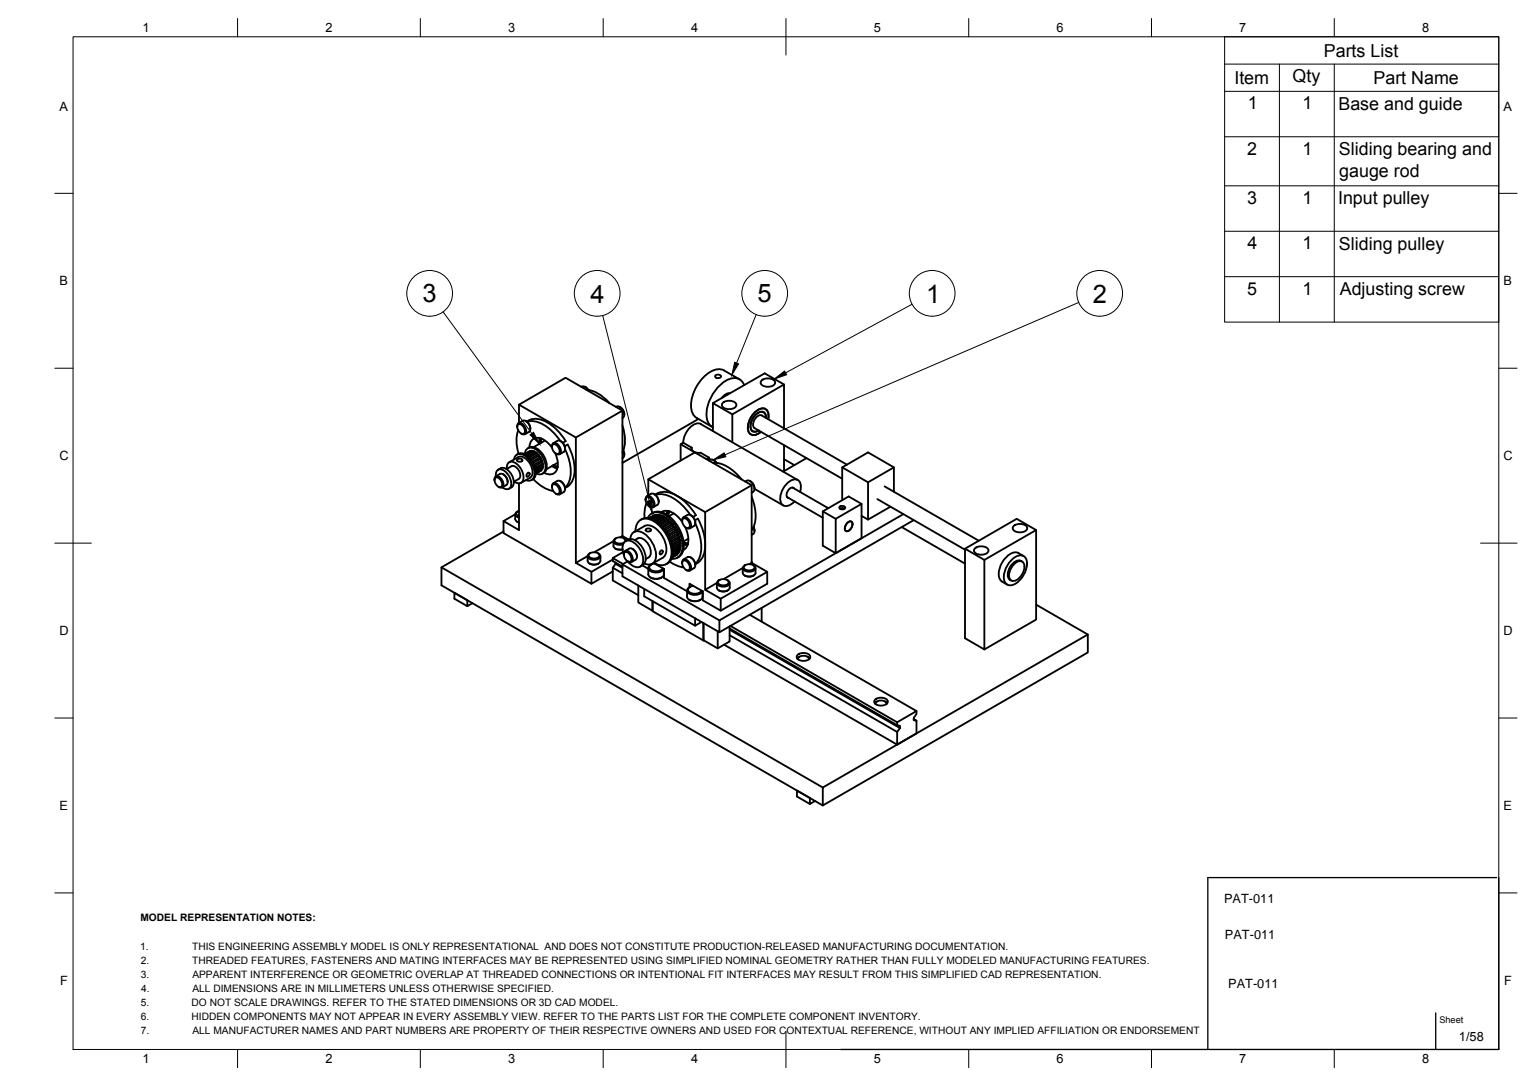
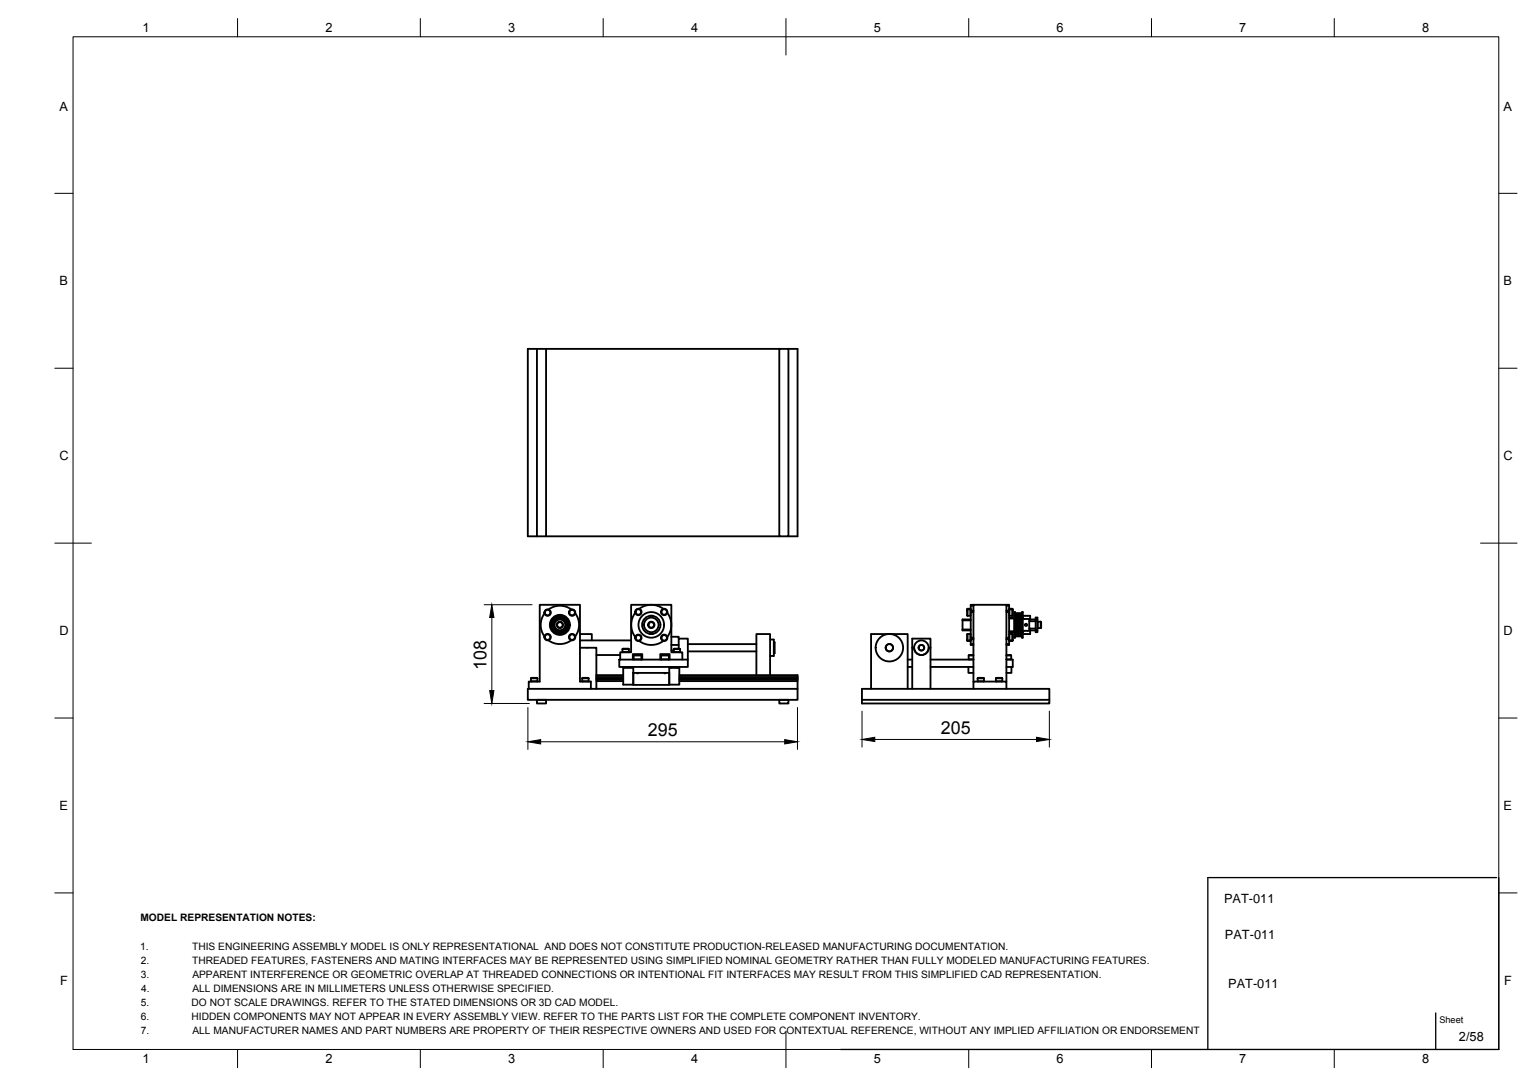
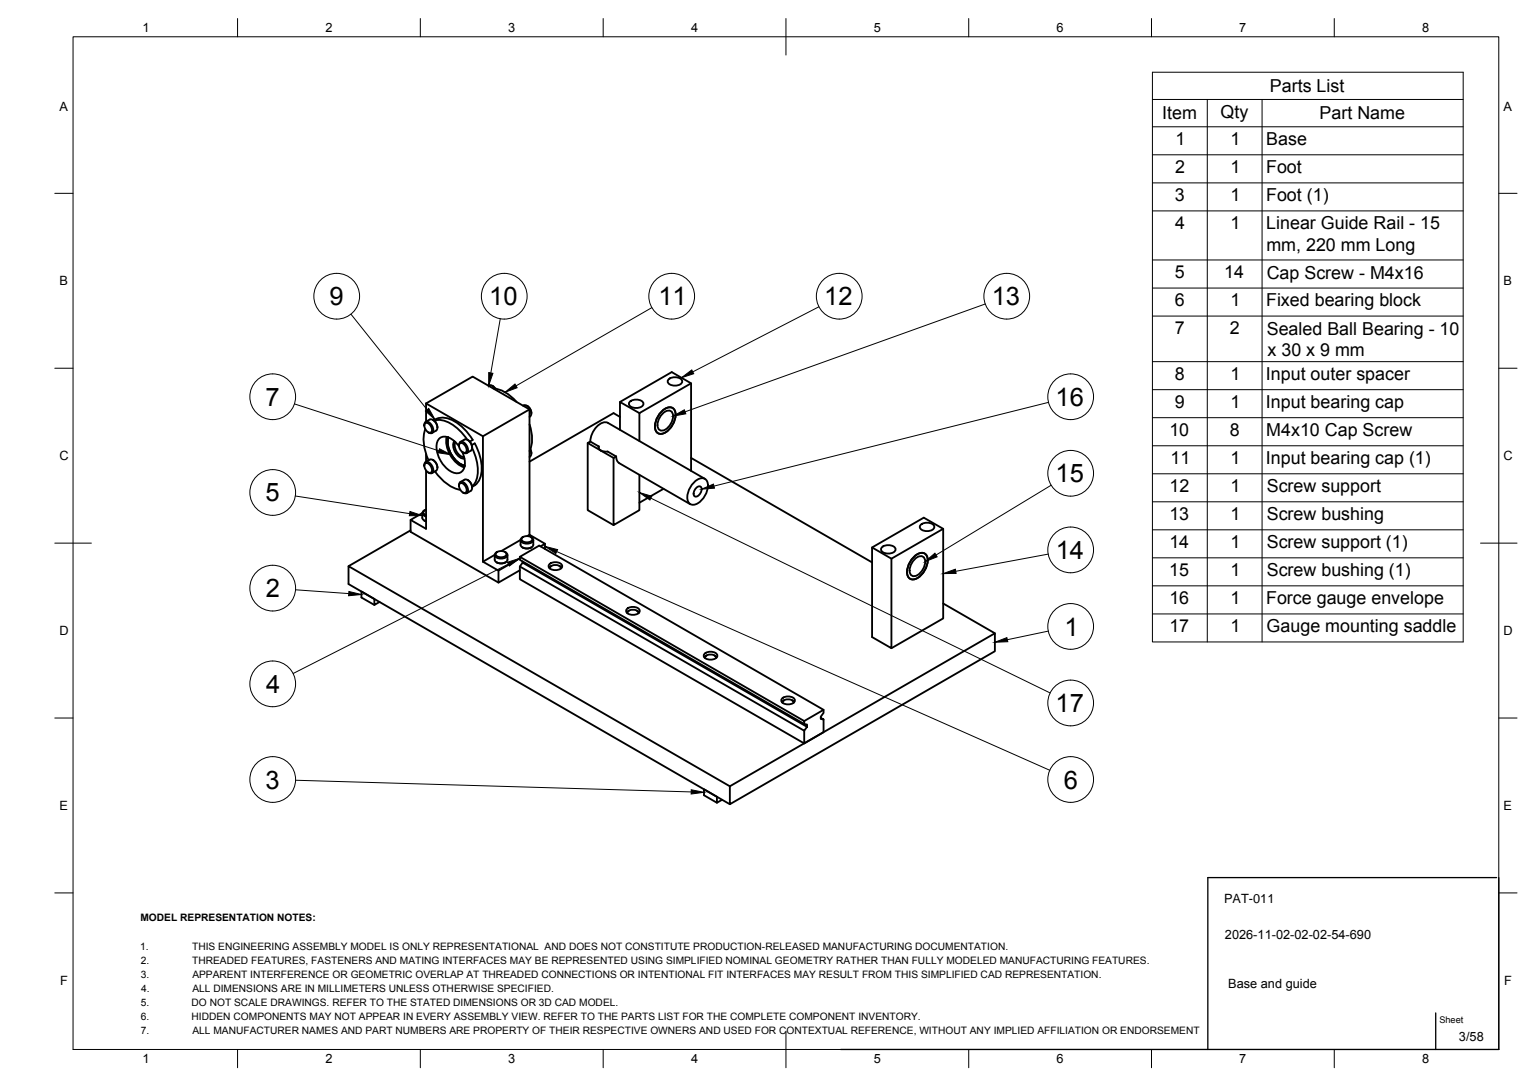
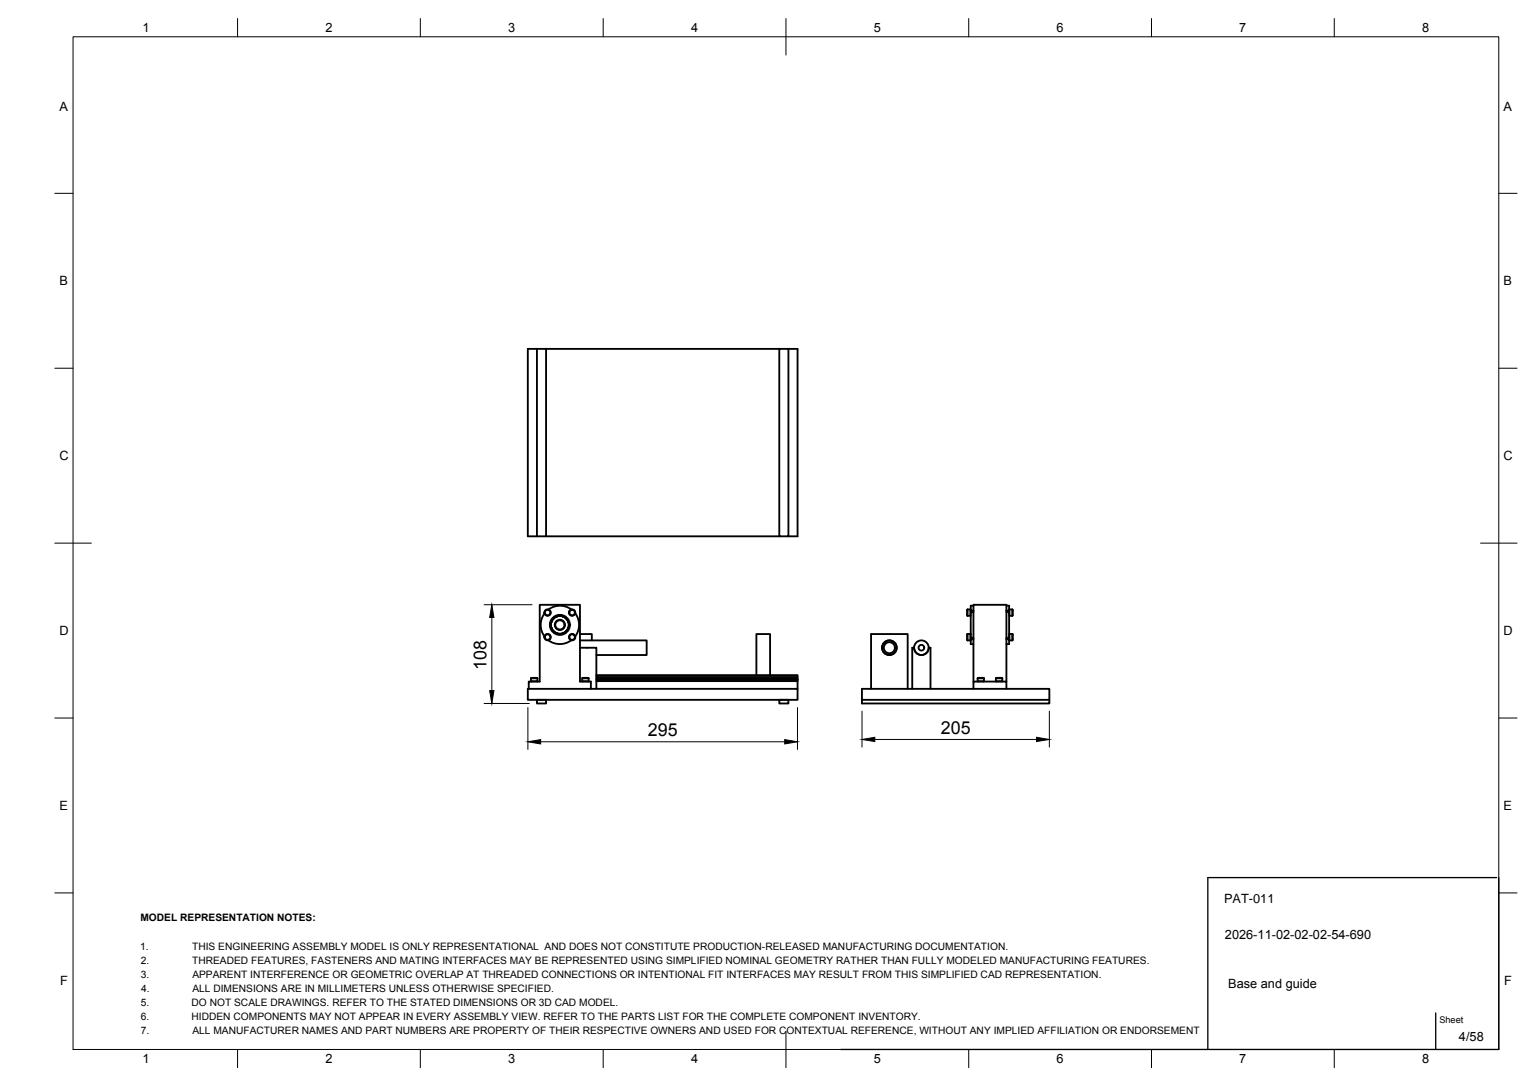
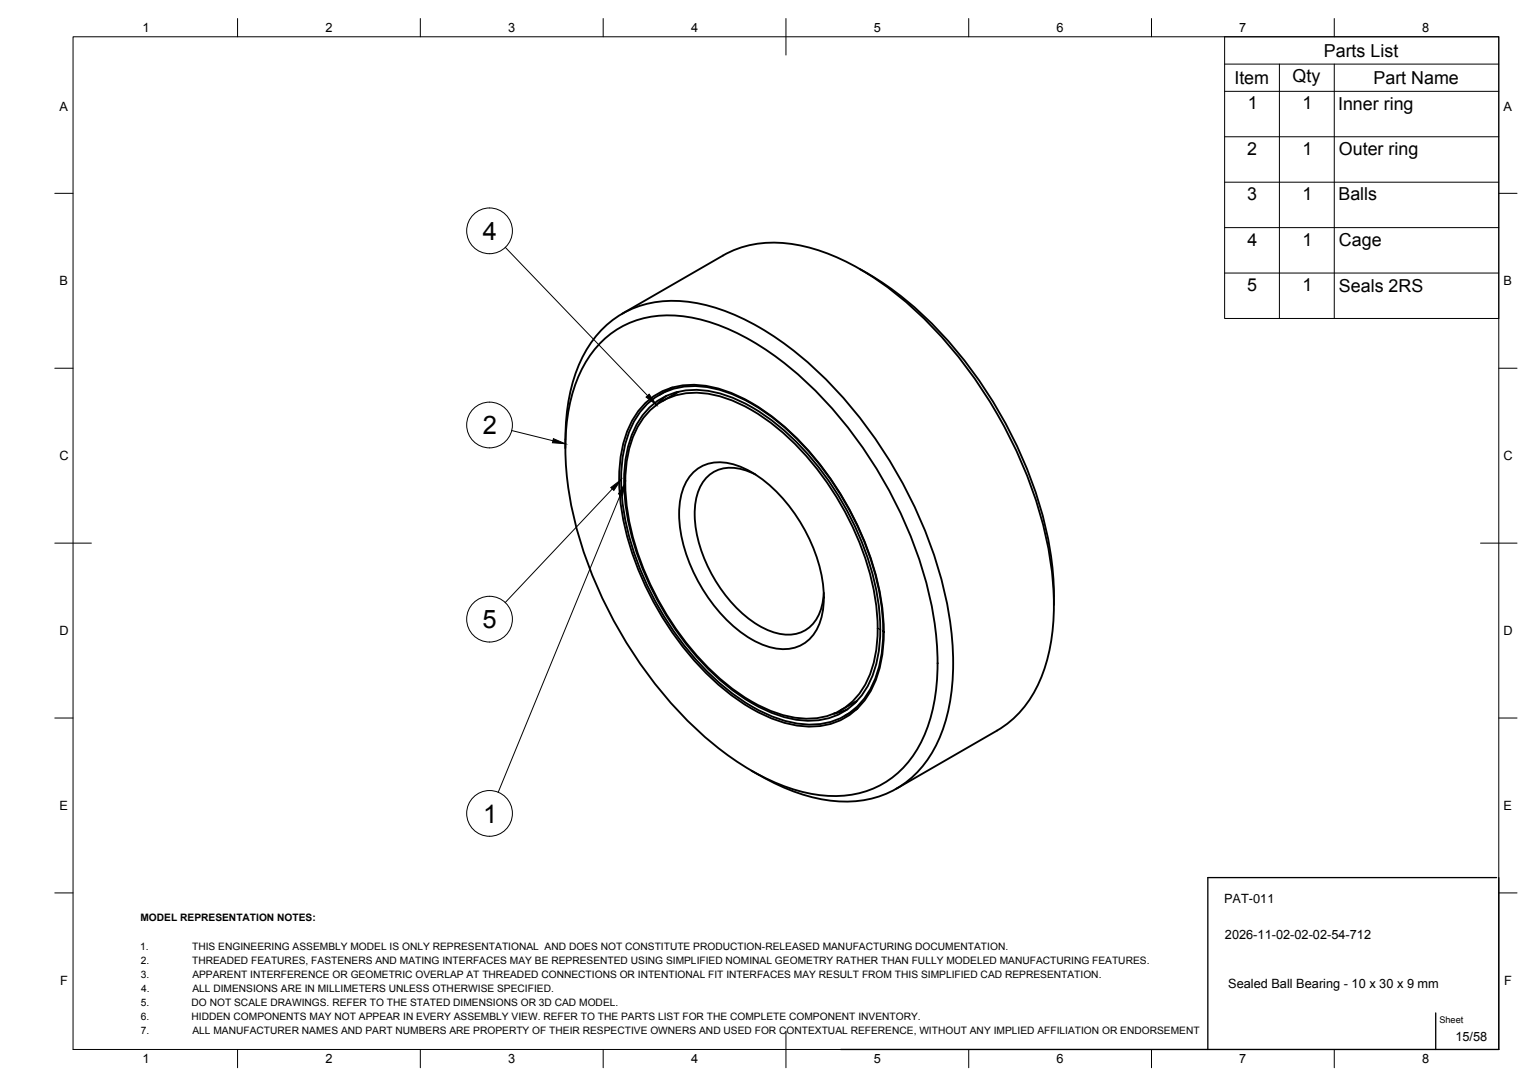
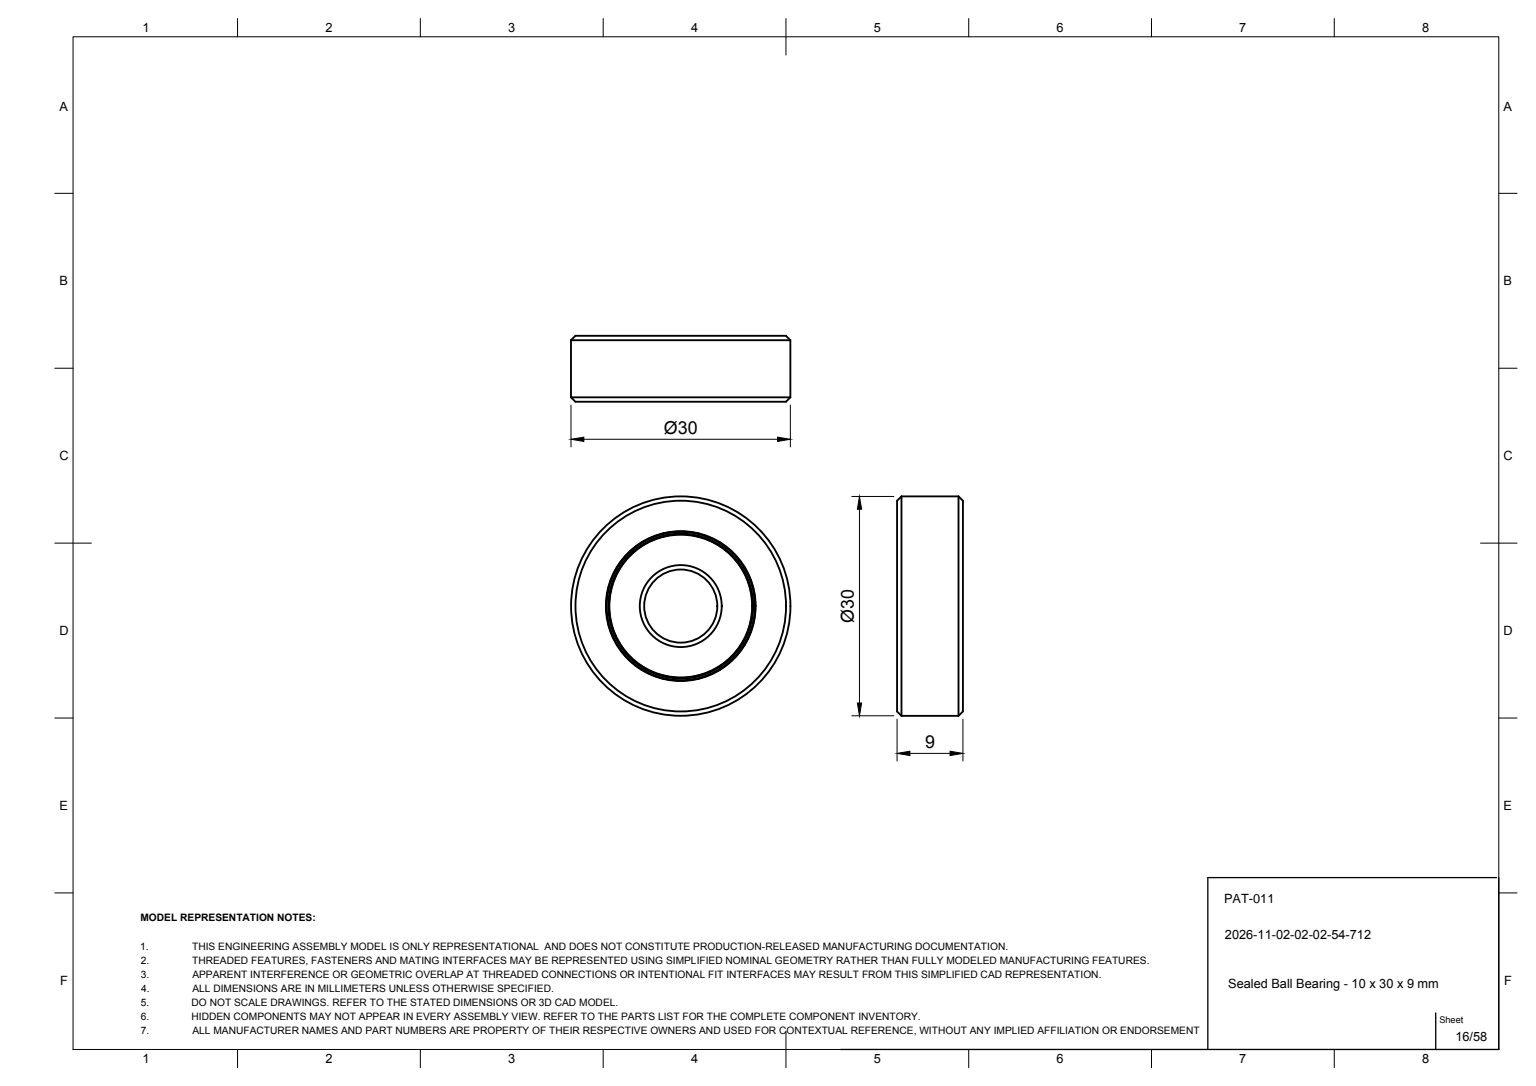
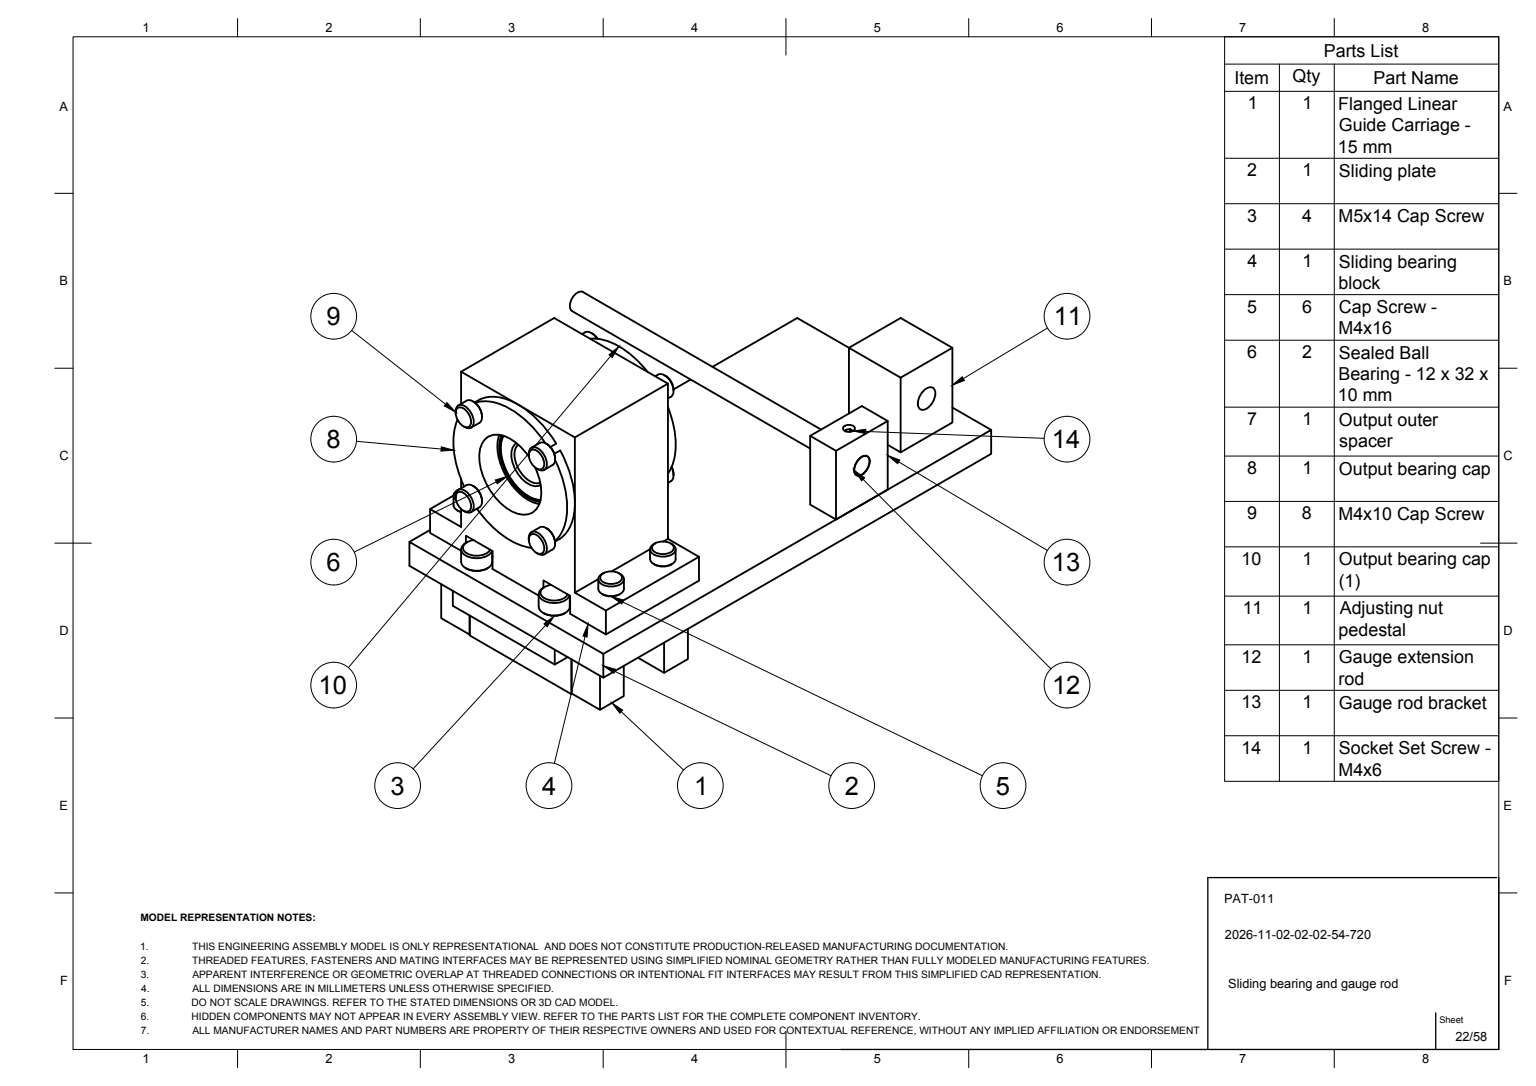
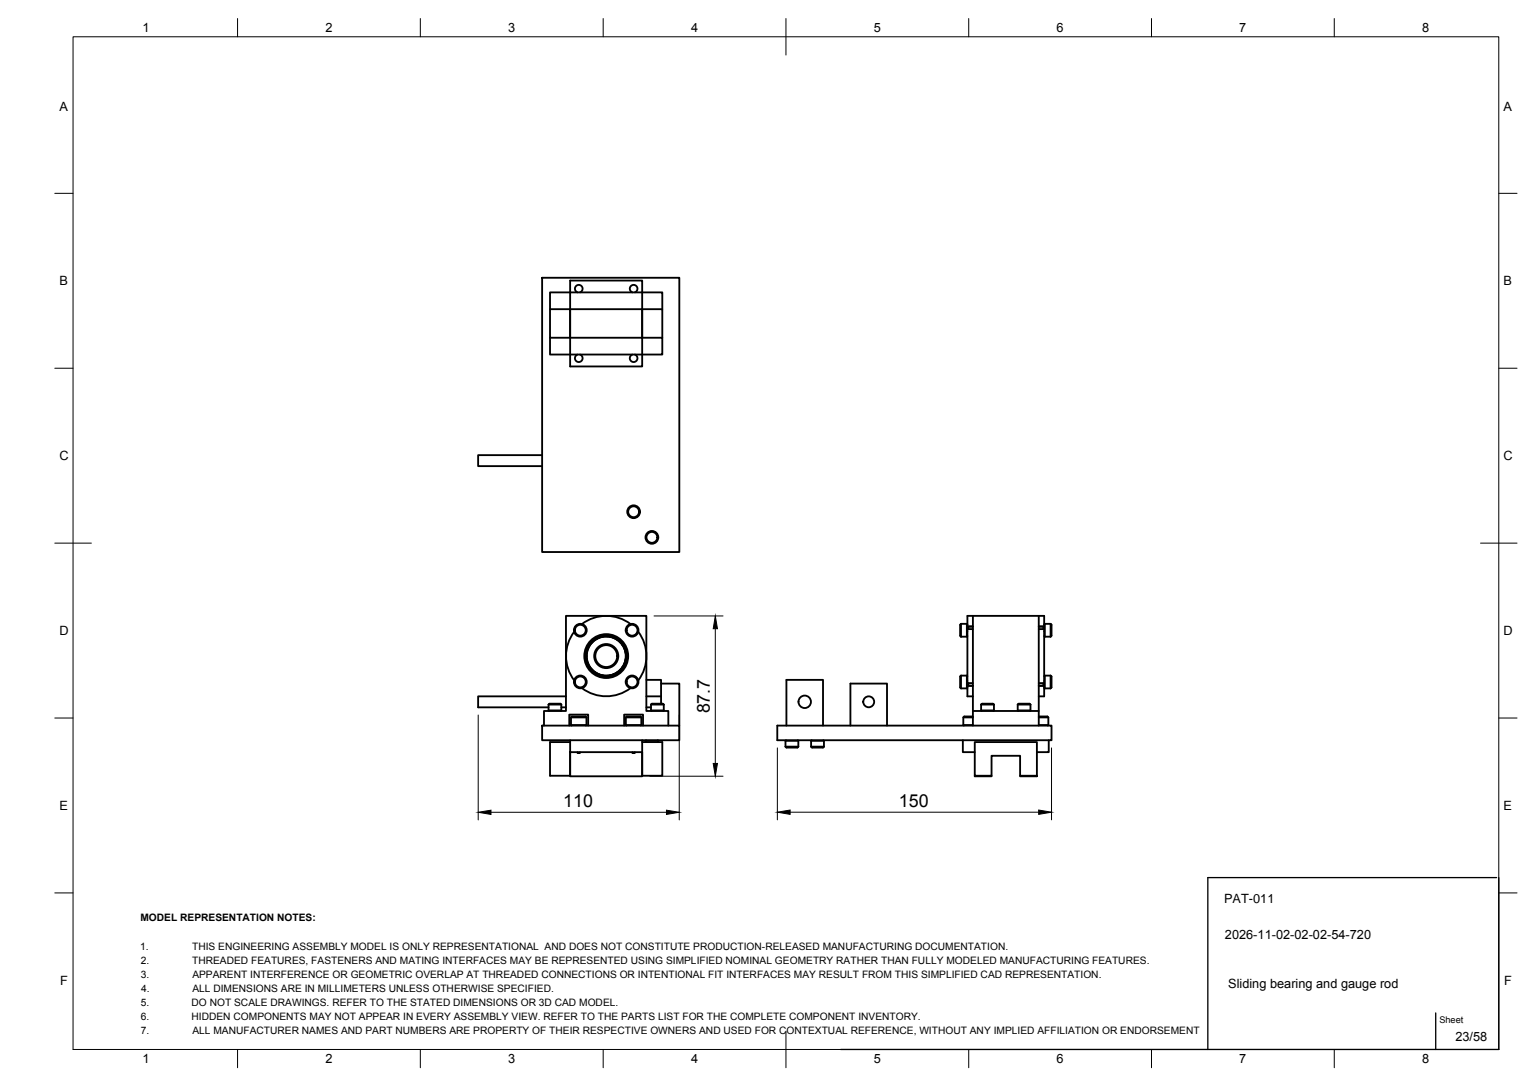
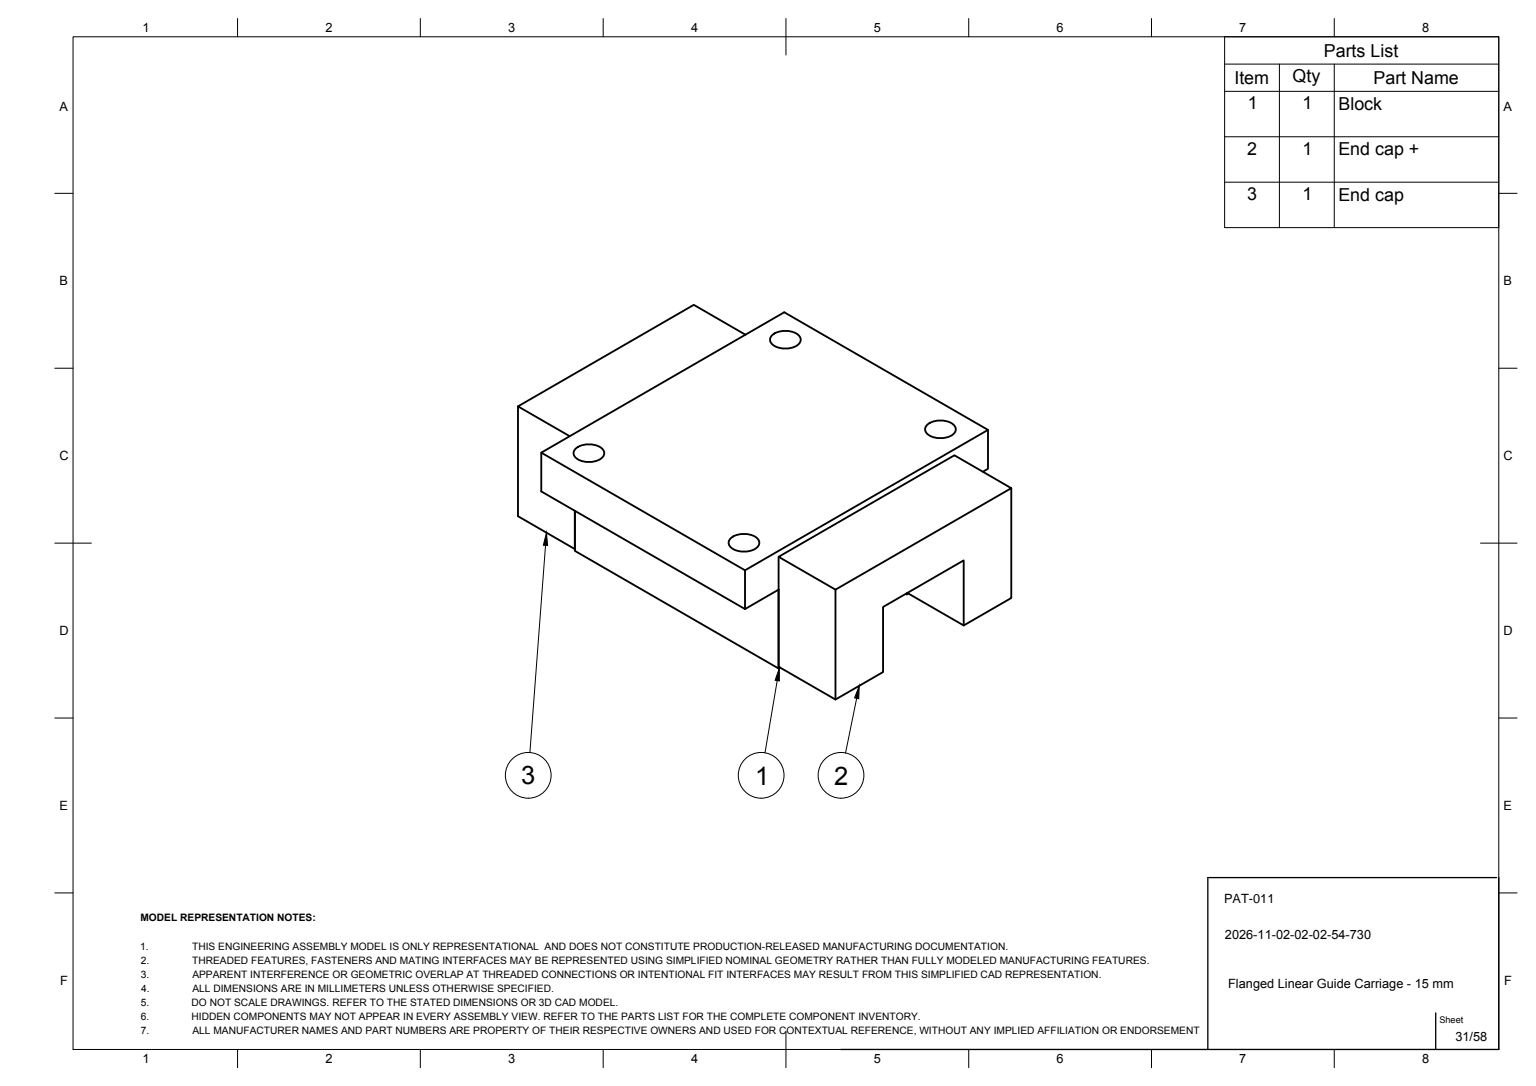
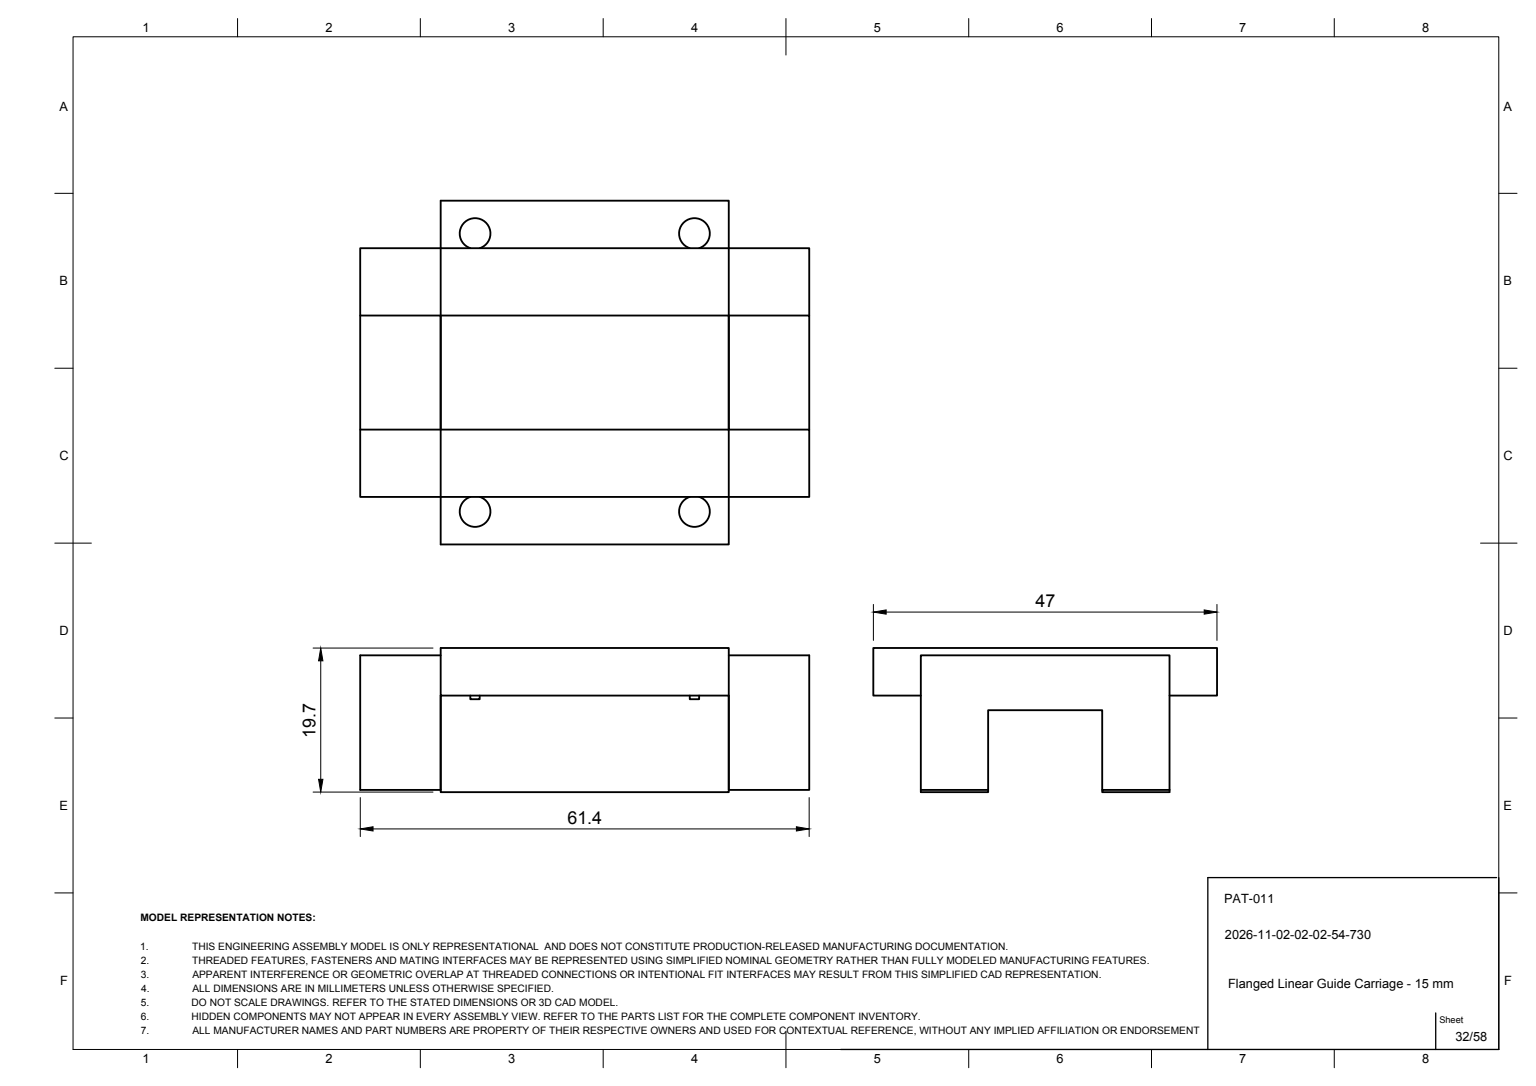
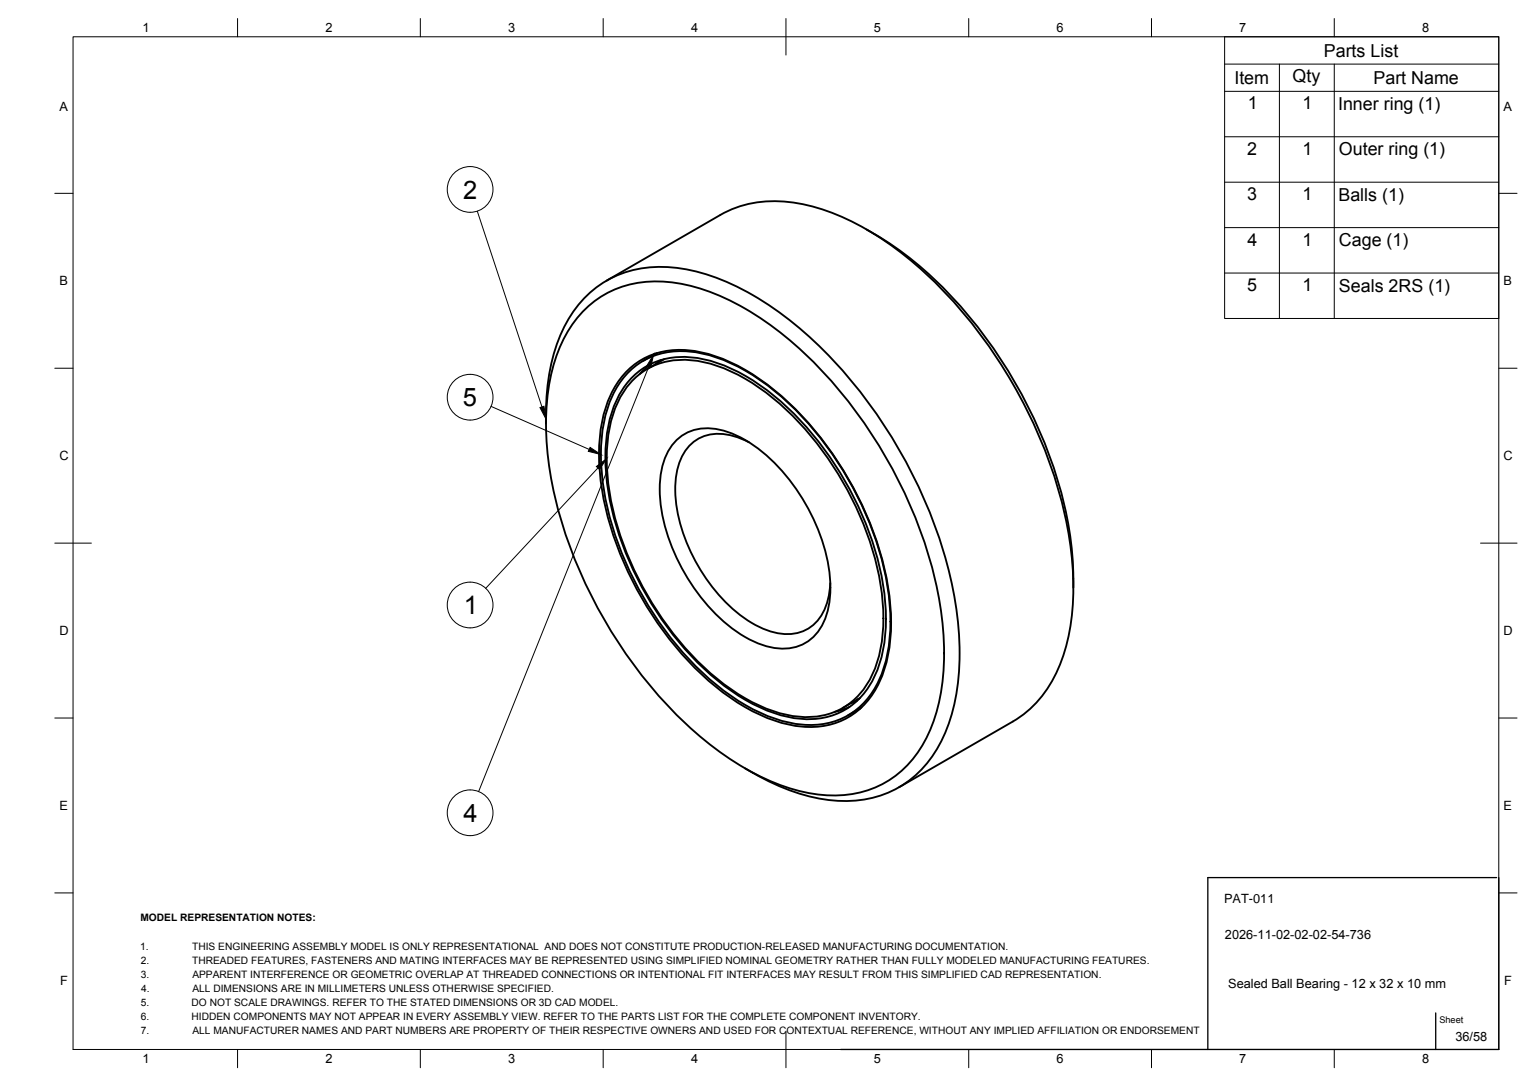
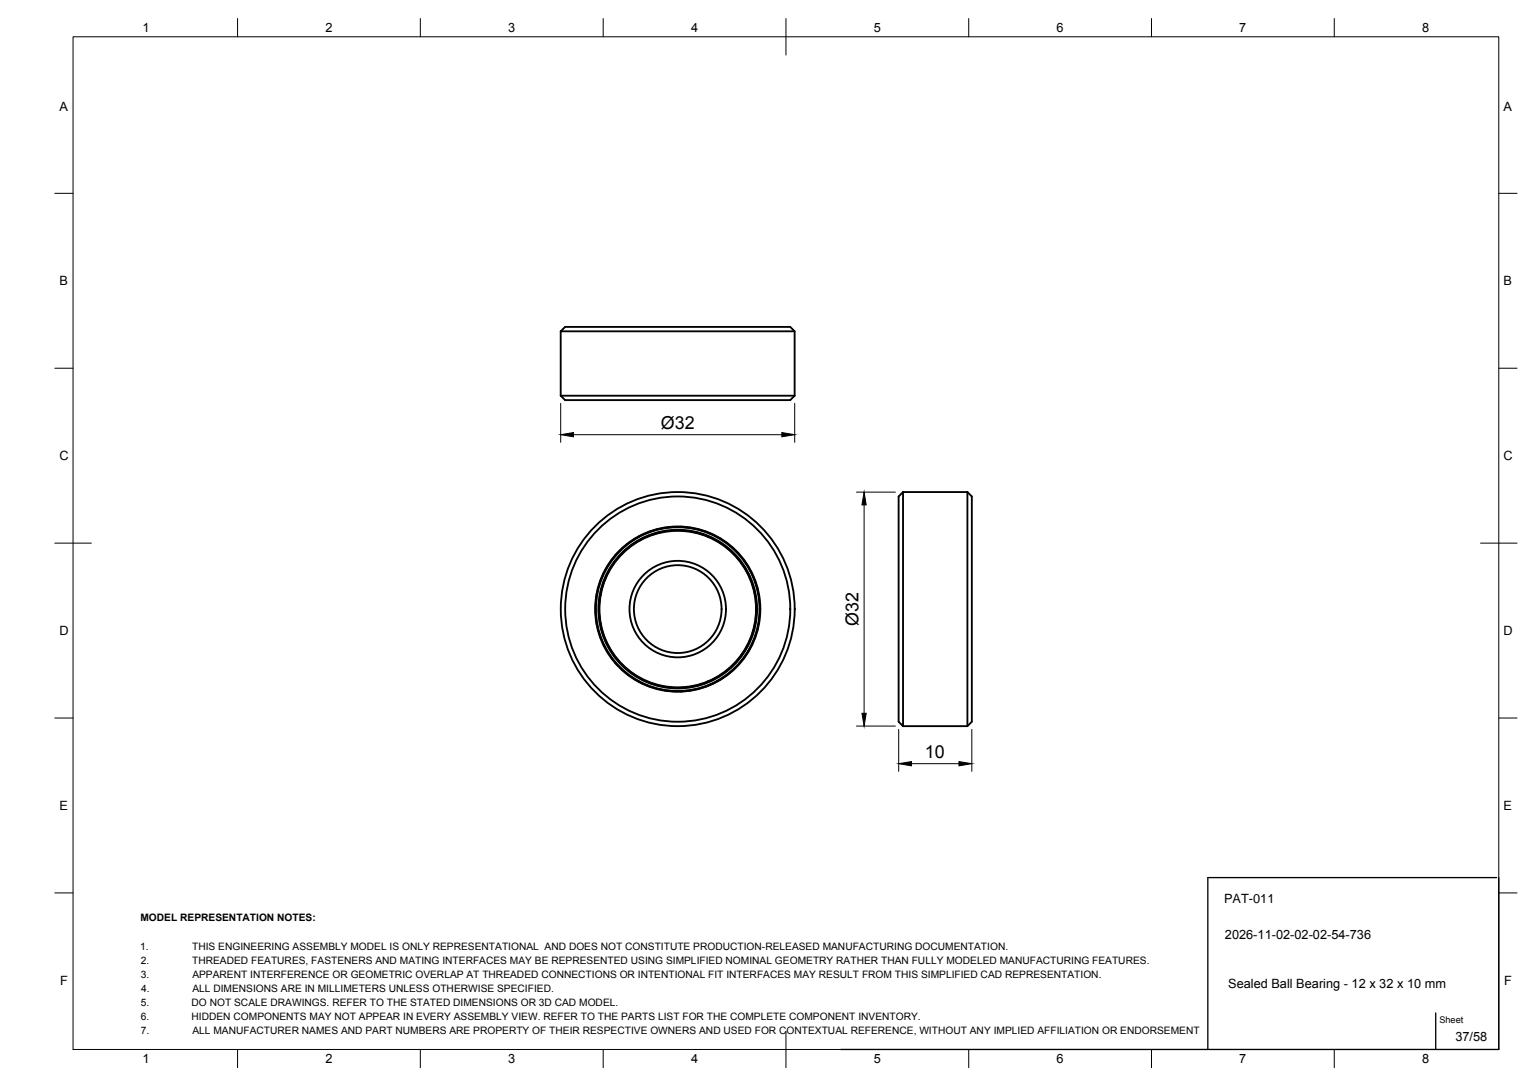
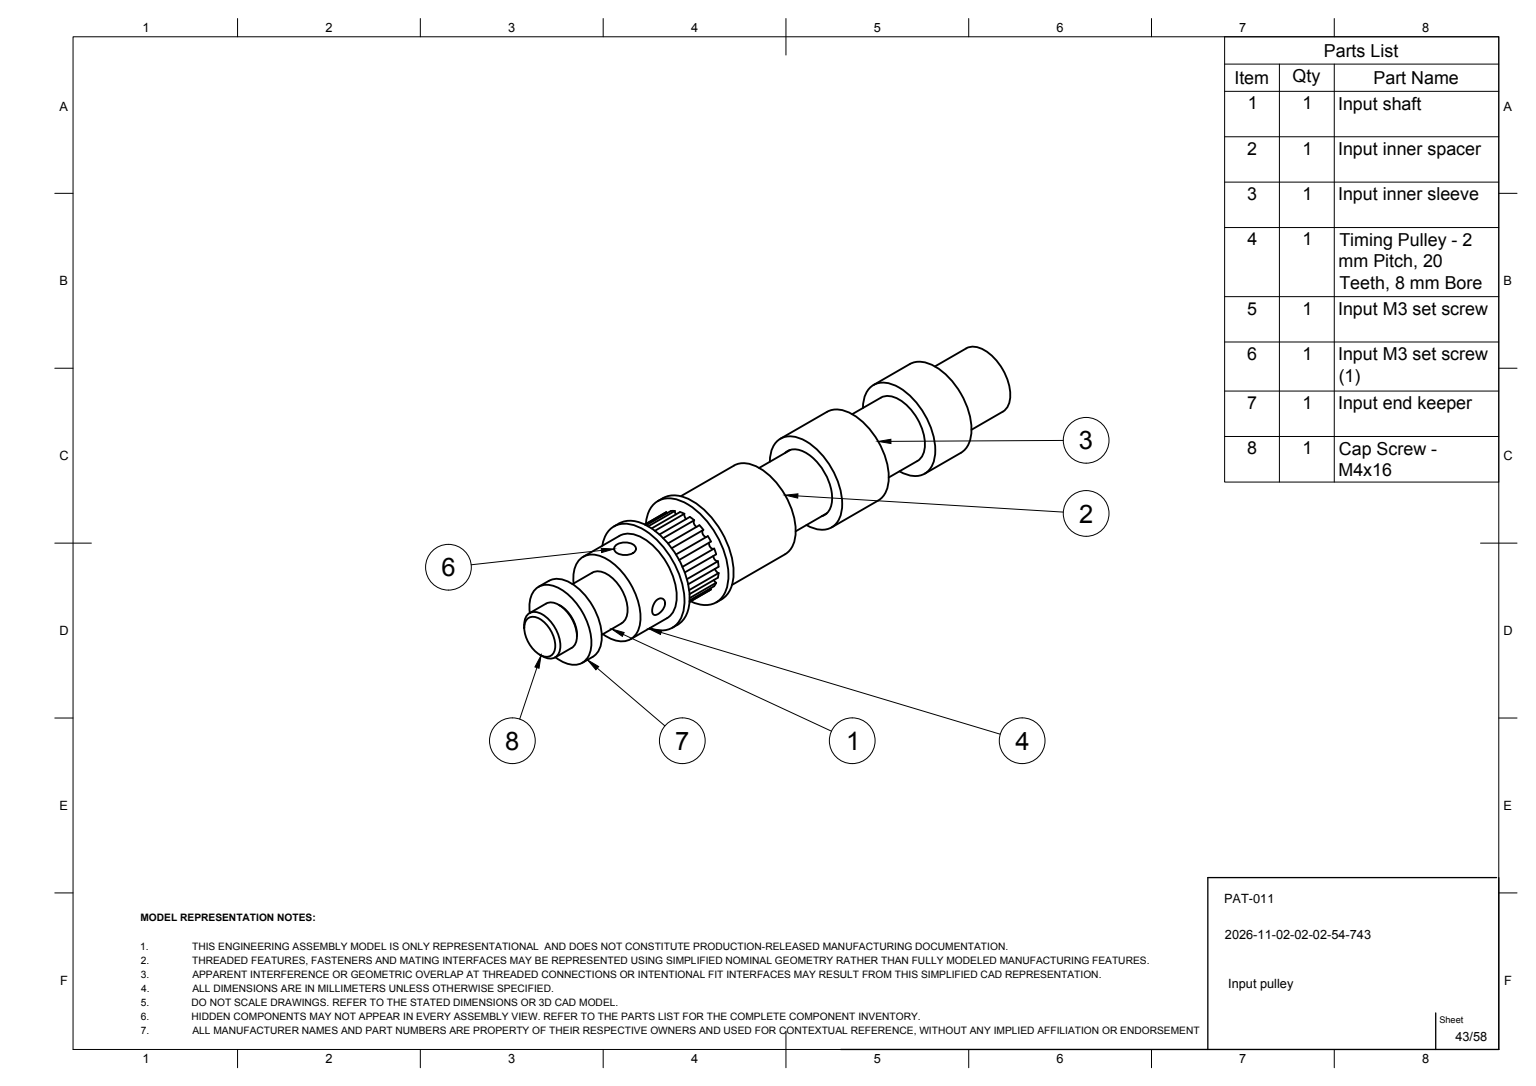
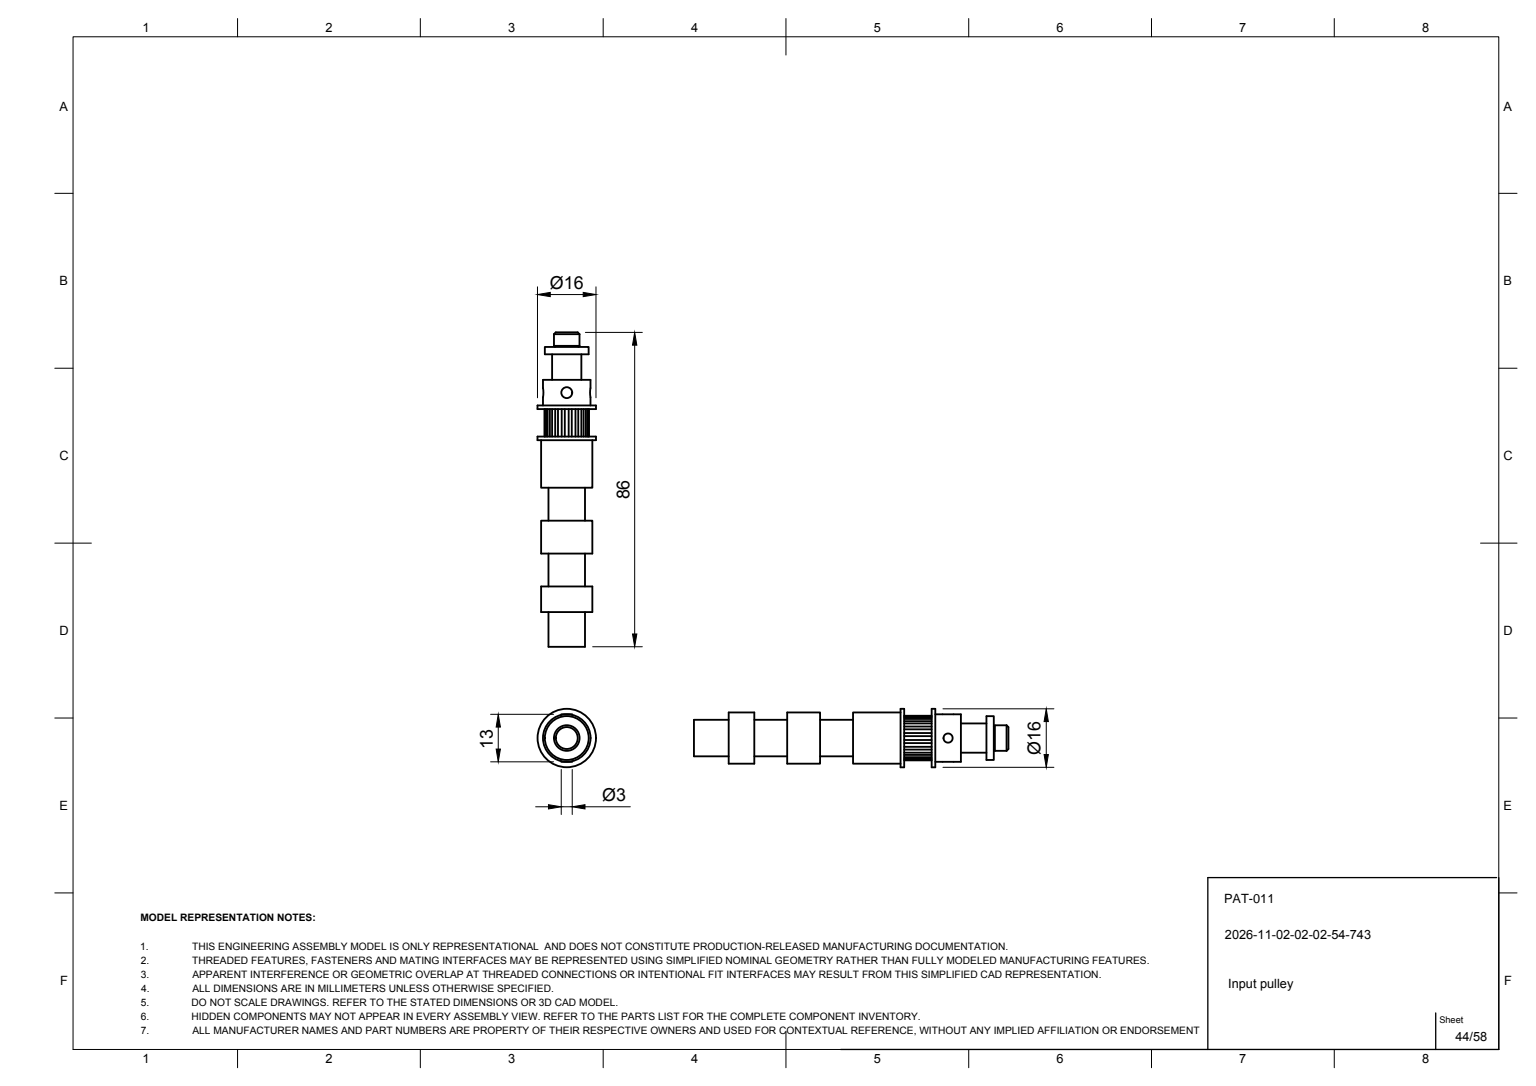
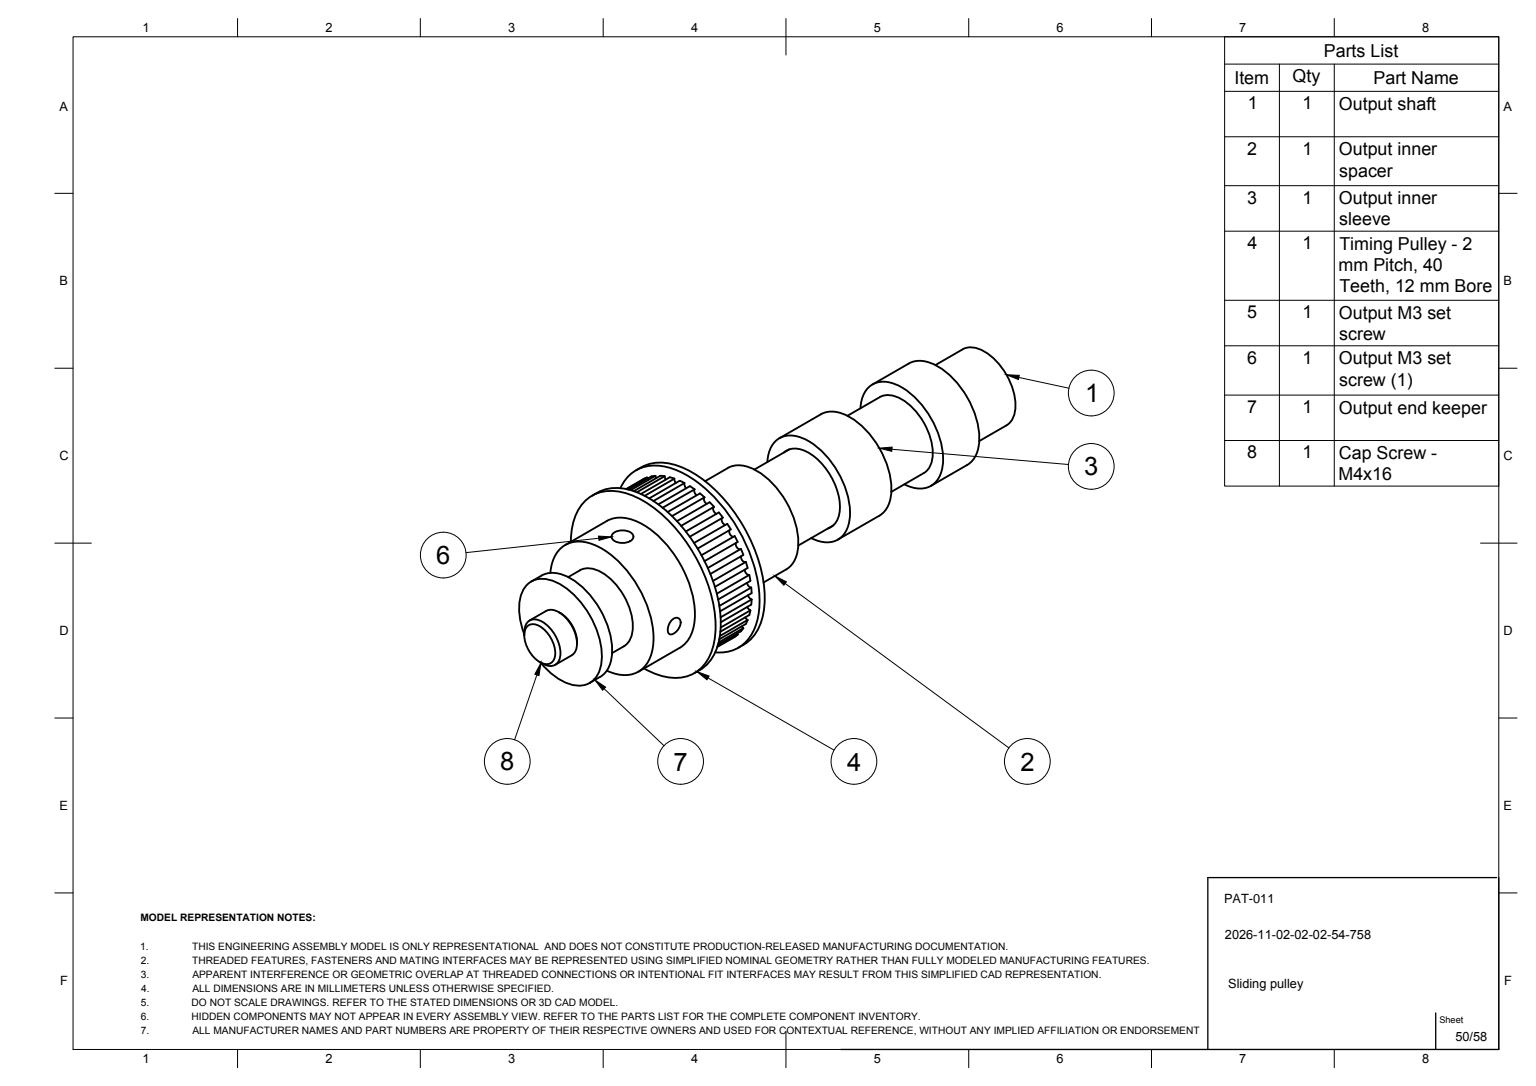
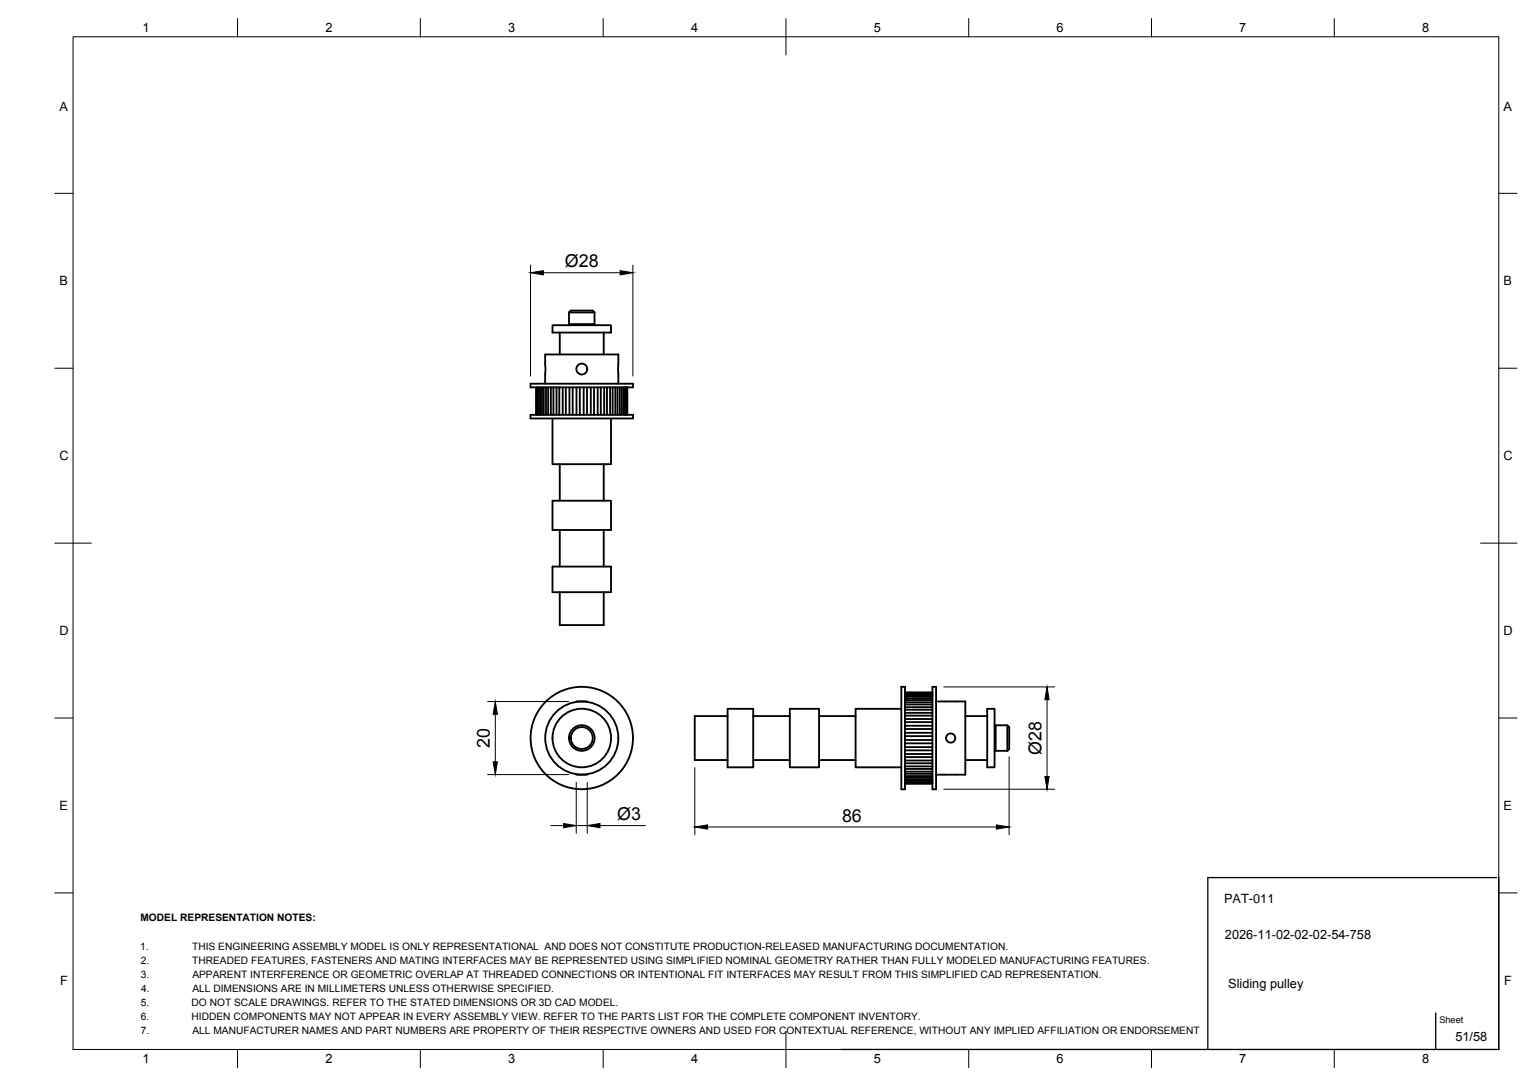
ISO-10303-21;
HEADER;
/* Generated by software containing ST-Developer
 * from STEP Tools, Inc. (www.steptools.com) 
 */

FILE_DESCRIPTION(
/* description */ ('Belt tension measurement rig'),
/* implementation_level */ '2;1');

FILE_NAME(
/* name */ 'PAT-011',
/* time_stamp */ '2026-10-28T03:24:44-07:00',
/* author */ (''),
/* organization */ (''),
/* preprocessor_version */ 'ST-DEVELOPER v20.2',
/* originating_system */ 'Autodesk Translation Framework v15.17.0.0',
/* authorisation */ '');

FILE_SCHEMA (('AUTOMOTIVE_DESIGN { 1 0 10303 214 3 1 1 }'));
ENDSEC;

DATA;
#10=MECHANICAL_DESIGN_GEOMETRIC_PRESENTATION_REPRESENTATION('',(#692,#693,
#694,#695,#696,#697,#698,#699,#700,#701,#702,#703,#704,#705,#706,#707,#708,
#709,#710,#711,#712,#713,#714,#715,#716,#717,#718,#719,#720,#721,#722,#723,
#724,#725,#726,#727,#728,#729,#730,#731,#732,#733,#734,#735,#736,#737,#738,
#739,#740,#741,#742,#743,#744,#745,#746,#747,#748,#749,#750,#751,#752,#753,
#754,#755,#756,#757,#758,#759,#760,#761),#23587);
#11=ORIENTED_CLOSED_SHELL('',*,#12235,.F.);
#12=ORIENTED_CLOSED_SHELL('',*,#12249,.F.);
#13=ORIENTED_CLOSED_SHELL('',*,#12266,.F.);
#14=BREP_WITH_VOIDS('Body1',#12236,(#11));
#15=BREP_WITH_VOIDS('Body1',#12250,(#12));
#16=BREP_WITH_VOIDS('Body1',#12265,(#13));
#17=ITEM_DEFINED_TRANSFORMATION($,$,#13222,#13350);
#18=ITEM_DEFINED_TRANSFORMATION($,$,#13242,#13351);
#19=ITEM_DEFINED_TRANSFORMATION($,$,#13262,#13352);
#20=ITEM_DEFINED_TRANSFORMATION($,$,#13279,#13353);
#21=ITEM_DEFINED_TRANSFORMATION($,$,#13333,#13354);
#22=ITEM_DEFINED_TRANSFORMATION($,$,#13565,#13626);
#23=ITEM_DEFINED_TRANSFORMATION($,$,#13604,#13627);
#24=ITEM_DEFINED_TRANSFORMATION($,$,#13615,#13628);
#25=ITEM_DEFINED_TRANSFORMATION($,$,#13654,#13776);
#26=ITEM_DEFINED_TRANSFORMATION($,$,#13674,#13777);
#27=ITEM_DEFINED_TRANSFORMATION($,$,#13694,#13778);
#28=ITEM_DEFINED_TRANSFORMATION($,$,#13709,#13779);
#29=ITEM_DEFINED_TRANSFORMATION($,$,#13759,#13780);
#30=ITEM_DEFINED_TRANSFORMATION($,$,#12878,#14359);
#31=ITEM_DEFINED_TRANSFORMATION($,$,#12941,#14360);
#32=ITEM_DEFINED_TRANSFORMATION($,$,#12948,#14361);
#33=ITEM_DEFINED_TRANSFORMATION($,$,#12955,#14362);
#34=ITEM_DEFINED_TRANSFORMATION($,$,#12993,#14363);
#35=ITEM_DEFINED_TRANSFORMATION($,$,#13002,#14364);
#36=ITEM_DEFINED_TRANSFORMATION($,$,#13036,#14365);
#37=ITEM_DEFINED_TRANSFORMATION($,$,#13070,#14366);
#38=ITEM_DEFINED_TRANSFORMATION($,$,#13094,#14367);
#39=ITEM_DEFINED_TRANSFORMATION($,$,#13103,#14368);
#40=ITEM_DEFINED_TRANSFORMATION($,$,#13127,#14369);
#41=ITEM_DEFINED_TRANSFORMATION($,$,#13136,#14370);
#42=ITEM_DEFINED_TRANSFORMATION($,$,#13145,#14371);
#43=ITEM_DEFINED_TRANSFORMATION($,$,#13178,#14372);
#44=ITEM_DEFINED_TRANSFORMATION($,$,#14333,#14373);
#45=ITEM_DEFINED_TRANSFORMATION($,$,#14333,#14374);
#46=ITEM_DEFINED_TRANSFORMATION($,$,#14333,#14375);
#47=ITEM_DEFINED_TRANSFORMATION($,$,#14333,#14376);
#48=ITEM_DEFINED_TRANSFORMATION($,$,#14333,#14377);
#49=ITEM_DEFINED_TRANSFORMATION($,$,#14333,#14378);
#50=ITEM_DEFINED_TRANSFORMATION($,$,#14333,#14379);
#51=ITEM_DEFINED_TRANSFORMATION($,$,#14333,#14380);
#52=ITEM_DEFINED_TRANSFORMATION($,$,#13221,#14381);
#53=ITEM_DEFINED_TRANSFORMATION($,$,#13221,#14382);
#54=ITEM_DEFINED_TRANSFORMATION($,$,#13781,#14383);
#55=ITEM_DEFINED_TRANSFORMATION($,$,#13781,#14384);
#56=ITEM_DEFINED_TRANSFORMATION($,$,#13781,#14385);
#57=ITEM_DEFINED_TRANSFORMATION($,$,#13781,#14386);
#58=ITEM_DEFINED_TRANSFORMATION($,$,#13781,#14387);
#59=ITEM_DEFINED_TRANSFORMATION($,$,#13781,#14388);
#60=ITEM_DEFINED_TRANSFORMATION($,$,#13781,#14389);
#61=ITEM_DEFINED_TRANSFORMATION($,$,#13781,#14390);
#62=ITEM_DEFINED_TRANSFORMATION($,$,#14333,#14391);
#63=ITEM_DEFINED_TRANSFORMATION($,$,#14333,#14392);
#64=ITEM_DEFINED_TRANSFORMATION($,$,#14333,#14393);
#65=ITEM_DEFINED_TRANSFORMATION($,$,#14333,#14394);
#66=ITEM_DEFINED_TRANSFORMATION($,$,#14333,#14395);
#67=ITEM_DEFINED_TRANSFORMATION($,$,#14333,#14396);
#68=ITEM_DEFINED_TRANSFORMATION($,$,#13806,#14397);
#69=ITEM_DEFINED_TRANSFORMATION($,$,#13828,#14398);
#70=ITEM_DEFINED_TRANSFORMATION($,$,#13841,#14399);
#71=ITEM_DEFINED_TRANSFORMATION($,$,#13850,#14400);
#72=ITEM_DEFINED_TRANSFORMATION($,$,#13856,#14401);
#73=ITEM_DEFINED_TRANSFORMATION($,$,#13862,#14402);
#74=ITEM_DEFINED_TRANSFORMATION($,$,#13871,#14403);
#75=ITEM_DEFINED_TRANSFORMATION($,$,#14333,#14404);
#76=ITEM_DEFINED_TRANSFORMATION($,$,#14014,#14405);
#77=ITEM_DEFINED_TRANSFORMATION($,$,#14032,#14406);
#78=ITEM_DEFINED_TRANSFORMATION($,$,#14041,#14407);
#79=ITEM_DEFINED_TRANSFORMATION($,$,#14050,#14408);
#80=ITEM_DEFINED_TRANSFORMATION($,$,#14056,#14409);
#81=ITEM_DEFINED_TRANSFORMATION($,$,#14062,#14410);
#82=ITEM_DEFINED_TRANSFORMATION($,$,#14071,#14411);
#83=ITEM_DEFINED_TRANSFORMATION($,$,#14333,#14412);
#84=ITEM_DEFINED_TRANSFORMATION($,$,#13356,#14479);
#85=ITEM_DEFINED_TRANSFORMATION($,$,#13393,#14480);
#86=ITEM_DEFINED_TRANSFORMATION($,$,#13447,#14481);
#87=ITEM_DEFINED_TRANSFORMATION($,$,#13456,#14482);
#88=ITEM_DEFINED_TRANSFORMATION($,$,#13490,#14483);
#89=ITEM_DEFINED_TRANSFORMATION($,$,#13524,#14484);
#90=ITEM_DEFINED_TRANSFORMATION($,$,#13542,#14485);
#91=ITEM_DEFINED_TRANSFORMATION($,$,#13548,#14486);
#92=ITEM_DEFINED_TRANSFORMATION($,$,#13564,#14487);
#93=ITEM_DEFINED_TRANSFORMATION($,$,#13629,#14488);
#94=ITEM_DEFINED_TRANSFORMATION($,$,#13629,#14489);
#95=ITEM_DEFINED_TRANSFORMATION($,$,#13629,#14490);
#96=ITEM_DEFINED_TRANSFORMATION($,$,#13629,#14491);
#97=ITEM_DEFINED_TRANSFORMATION($,$,#14333,#14492);
#98=ITEM_DEFINED_TRANSFORMATION($,$,#14333,#14493);
#99=ITEM_DEFINED_TRANSFORMATION($,$,#14333,#14494);
#100=ITEM_DEFINED_TRANSFORMATION($,$,#14333,#14495);
#101=ITEM_DEFINED_TRANSFORMATION($,$,#13653,#14496);
#102=ITEM_DEFINED_TRANSFORMATION($,$,#13653,#14497);
#103=ITEM_DEFINED_TRANSFORMATION($,$,#13781,#14498);
#104=ITEM_DEFINED_TRANSFORMATION($,$,#13781,#14499);
#105=ITEM_DEFINED_TRANSFORMATION($,$,#13781,#14500);
#106=ITEM_DEFINED_TRANSFORMATION($,$,#13781,#14501);
#107=ITEM_DEFINED_TRANSFORMATION($,$,#13781,#14502);
#108=ITEM_DEFINED_TRANSFORMATION($,$,#13781,#14503);
#109=ITEM_DEFINED_TRANSFORMATION($,$,#13781,#14504);
#110=ITEM_DEFINED_TRANSFORMATION($,$,#13781,#14505);
#111=ITEM_DEFINED_TRANSFORMATION($,$,#14333,#14506);
#112=ITEM_DEFINED_TRANSFORMATION($,$,#14333,#14507);
#113=ITEM_DEFINED_TRANSFORMATION($,$,#14462,#14508);
#114=ITEM_DEFINED_TRANSFORMATION($,$,#14414,#14509);
#115=ITEM_DEFINED_TRANSFORMATION($,$,#14448,#14510);
#116=ITEM_DEFINED_TRANSFORMATION($,$,#14462,#14511);
#117=ITEM_DEFINED_TRANSFORMATION($,$,#12877,#14512);
#118=ITEM_DEFINED_TRANSFORMATION($,$,#13355,#14513);
#119=ITEM_DEFINED_TRANSFORMATION($,$,#13805,#14514);
#120=ITEM_DEFINED_TRANSFORMATION($,$,#14013,#14515);
#121=ITEM_DEFINED_TRANSFORMATION($,$,#14413,#14516);
#122=(
REPRESENTATION_RELATIONSHIP($,$,#23842,#23841)
REPRESENTATION_RELATIONSHIP_WITH_TRANSFORMATION(#17)
SHAPE_REPRESENTATION_RELATIONSHIP()
);
#123=(
REPRESENTATION_RELATIONSHIP($,$,#23843,#23841)
REPRESENTATION_RELATIONSHIP_WITH_TRANSFORMATION(#18)
SHAPE_REPRESENTATION_RELATIONSHIP()
);
#124=(
REPRESENTATION_RELATIONSHIP($,$,#23844,#23841)
REPRESENTATION_RELATIONSHIP_WITH_TRANSFORMATION(#19)
SHAPE_REPRESENTATION_RELATIONSHIP()
);
#125=(
REPRESENTATION_RELATIONSHIP($,$,#23845,#23841)
REPRESENTATION_RELATIONSHIP_WITH_TRANSFORMATION(#20)
SHAPE_REPRESENTATION_RELATIONSHIP()
);
#126=(
REPRESENTATION_RELATIONSHIP($,$,#23846,#23841)
REPRESENTATION_RELATIONSHIP_WITH_TRANSFORMATION(#21)
SHAPE_REPRESENTATION_RELATIONSHIP()
);
#127=(
REPRESENTATION_RELATIONSHIP($,$,#23857,#23856)
REPRESENTATION_RELATIONSHIP_WITH_TRANSFORMATION(#22)
SHAPE_REPRESENTATION_RELATIONSHIP()
);
#128=(
REPRESENTATION_RELATIONSHIP($,$,#23858,#23856)
REPRESENTATION_RELATIONSHIP_WITH_TRANSFORMATION(#23)
SHAPE_REPRESENTATION_RELATIONSHIP()
);
#129=(
REPRESENTATION_RELATIONSHIP($,$,#23859,#23856)
REPRESENTATION_RELATIONSHIP_WITH_TRANSFORMATION(#24)
SHAPE_REPRESENTATION_RELATIONSHIP()
);
#130=(
REPRESENTATION_RELATIONSHIP($,$,#23862,#23861)
REPRESENTATION_RELATIONSHIP_WITH_TRANSFORMATION(#25)
SHAPE_REPRESENTATION_RELATIONSHIP()
);
#131=(
REPRESENTATION_RELATIONSHIP($,$,#23863,#23861)
REPRESENTATION_RELATIONSHIP_WITH_TRANSFORMATION(#26)
SHAPE_REPRESENTATION_RELATIONSHIP()
);
#132=(
REPRESENTATION_RELATIONSHIP($,$,#23864,#23861)
REPRESENTATION_RELATIONSHIP_WITH_TRANSFORMATION(#27)
SHAPE_REPRESENTATION_RELATIONSHIP()
);
#133=(
REPRESENTATION_RELATIONSHIP($,$,#23865,#23861)
REPRESENTATION_RELATIONSHIP_WITH_TRANSFORMATION(#28)
SHAPE_REPRESENTATION_RELATIONSHIP()
);
#134=(
REPRESENTATION_RELATIONSHIP($,$,#23866,#23861)
REPRESENTATION_RELATIONSHIP_WITH_TRANSFORMATION(#29)
SHAPE_REPRESENTATION_RELATIONSHIP()
);
#135=(
REPRESENTATION_RELATIONSHIP($,$,#23827,#23826)
REPRESENTATION_RELATIONSHIP_WITH_TRANSFORMATION(#30)
SHAPE_REPRESENTATION_RELATIONSHIP()
);
#136=(
REPRESENTATION_RELATIONSHIP($,$,#23828,#23826)
REPRESENTATION_RELATIONSHIP_WITH_TRANSFORMATION(#31)
SHAPE_REPRESENTATION_RELATIONSHIP()
);
#137=(
REPRESENTATION_RELATIONSHIP($,$,#23829,#23826)
REPRESENTATION_RELATIONSHIP_WITH_TRANSFORMATION(#32)
SHAPE_REPRESENTATION_RELATIONSHIP()
);
#138=(
REPRESENTATION_RELATIONSHIP($,$,#23830,#23826)
REPRESENTATION_RELATIONSHIP_WITH_TRANSFORMATION(#33)
SHAPE_REPRESENTATION_RELATIONSHIP()
);
#139=(
REPRESENTATION_RELATIONSHIP($,$,#23831,#23826)
REPRESENTATION_RELATIONSHIP_WITH_TRANSFORMATION(#34)
SHAPE_REPRESENTATION_RELATIONSHIP()
);
#140=(
REPRESENTATION_RELATIONSHIP($,$,#23832,#23826)
REPRESENTATION_RELATIONSHIP_WITH_TRANSFORMATION(#35)
SHAPE_REPRESENTATION_RELATIONSHIP()
);
#141=(
REPRESENTATION_RELATIONSHIP($,$,#23833,#23826)
REPRESENTATION_RELATIONSHIP_WITH_TRANSFORMATION(#36)
SHAPE_REPRESENTATION_RELATIONSHIP()
);
#142=(
REPRESENTATION_RELATIONSHIP($,$,#23834,#23826)
REPRESENTATION_RELATIONSHIP_WITH_TRANSFORMATION(#37)
SHAPE_REPRESENTATION_RELATIONSHIP()
);
#143=(
REPRESENTATION_RELATIONSHIP($,$,#23835,#23826)
REPRESENTATION_RELATIONSHIP_WITH_TRANSFORMATION(#38)
SHAPE_REPRESENTATION_RELATIONSHIP()
);
#144=(
REPRESENTATION_RELATIONSHIP($,$,#23836,#23826)
REPRESENTATION_RELATIONSHIP_WITH_TRANSFORMATION(#39)
SHAPE_REPRESENTATION_RELATIONSHIP()
);
#145=(
REPRESENTATION_RELATIONSHIP($,$,#23837,#23826)
REPRESENTATION_RELATIONSHIP_WITH_TRANSFORMATION(#40)
SHAPE_REPRESENTATION_RELATIONSHIP()
);
#146=(
REPRESENTATION_RELATIONSHIP($,$,#23838,#23826)
REPRESENTATION_RELATIONSHIP_WITH_TRANSFORMATION(#41)
SHAPE_REPRESENTATION_RELATIONSHIP()
);
#147=(
REPRESENTATION_RELATIONSHIP($,$,#23839,#23826)
REPRESENTATION_RELATIONSHIP_WITH_TRANSFORMATION(#42)
SHAPE_REPRESENTATION_RELATIONSHIP()
);
#148=(
REPRESENTATION_RELATIONSHIP($,$,#23840,#23826)
REPRESENTATION_RELATIONSHIP_WITH_TRANSFORMATION(#43)
SHAPE_REPRESENTATION_RELATIONSHIP()
);
#149=(
REPRESENTATION_RELATIONSHIP($,$,#23884,#23826)
REPRESENTATION_RELATIONSHIP_WITH_TRANSFORMATION(#44)
SHAPE_REPRESENTATION_RELATIONSHIP()
);
#150=(
REPRESENTATION_RELATIONSHIP($,$,#23884,#23826)
REPRESENTATION_RELATIONSHIP_WITH_TRANSFORMATION(#45)
SHAPE_REPRESENTATION_RELATIONSHIP()
);
#151=(
REPRESENTATION_RELATIONSHIP($,$,#23884,#23826)
REPRESENTATION_RELATIONSHIP_WITH_TRANSFORMATION(#46)
SHAPE_REPRESENTATION_RELATIONSHIP()
);
#152=(
REPRESENTATION_RELATIONSHIP($,$,#23884,#23826)
REPRESENTATION_RELATIONSHIP_WITH_TRANSFORMATION(#47)
SHAPE_REPRESENTATION_RELATIONSHIP()
);
#153=(
REPRESENTATION_RELATIONSHIP($,$,#23884,#23826)
REPRESENTATION_RELATIONSHIP_WITH_TRANSFORMATION(#48)
SHAPE_REPRESENTATION_RELATIONSHIP()
);
#154=(
REPRESENTATION_RELATIONSHIP($,$,#23884,#23826)
REPRESENTATION_RELATIONSHIP_WITH_TRANSFORMATION(#49)
SHAPE_REPRESENTATION_RELATIONSHIP()
);
#155=(
REPRESENTATION_RELATIONSHIP($,$,#23884,#23826)
REPRESENTATION_RELATIONSHIP_WITH_TRANSFORMATION(#50)
SHAPE_REPRESENTATION_RELATIONSHIP()
);
#156=(
REPRESENTATION_RELATIONSHIP($,$,#23884,#23826)
REPRESENTATION_RELATIONSHIP_WITH_TRANSFORMATION(#51)
SHAPE_REPRESENTATION_RELATIONSHIP()
);
#157=(
REPRESENTATION_RELATIONSHIP($,$,#23841,#23826)
REPRESENTATION_RELATIONSHIP_WITH_TRANSFORMATION(#52)
SHAPE_REPRESENTATION_RELATIONSHIP()
);
#158=(
REPRESENTATION_RELATIONSHIP($,$,#23841,#23826)
REPRESENTATION_RELATIONSHIP_WITH_TRANSFORMATION(#53)
SHAPE_REPRESENTATION_RELATIONSHIP()
);
#159=(
REPRESENTATION_RELATIONSHIP($,$,#23867,#23826)
REPRESENTATION_RELATIONSHIP_WITH_TRANSFORMATION(#54)
SHAPE_REPRESENTATION_RELATIONSHIP()
);
#160=(
REPRESENTATION_RELATIONSHIP($,$,#23867,#23826)
REPRESENTATION_RELATIONSHIP_WITH_TRANSFORMATION(#55)
SHAPE_REPRESENTATION_RELATIONSHIP()
);
#161=(
REPRESENTATION_RELATIONSHIP($,$,#23867,#23826)
REPRESENTATION_RELATIONSHIP_WITH_TRANSFORMATION(#56)
SHAPE_REPRESENTATION_RELATIONSHIP()
);
#162=(
REPRESENTATION_RELATIONSHIP($,$,#23867,#23826)
REPRESENTATION_RELATIONSHIP_WITH_TRANSFORMATION(#57)
SHAPE_REPRESENTATION_RELATIONSHIP()
);
#163=(
REPRESENTATION_RELATIONSHIP($,$,#23867,#23826)
REPRESENTATION_RELATIONSHIP_WITH_TRANSFORMATION(#58)
SHAPE_REPRESENTATION_RELATIONSHIP()
);
#164=(
REPRESENTATION_RELATIONSHIP($,$,#23867,#23826)
REPRESENTATION_RELATIONSHIP_WITH_TRANSFORMATION(#59)
SHAPE_REPRESENTATION_RELATIONSHIP()
);
#165=(
REPRESENTATION_RELATIONSHIP($,$,#23867,#23826)
REPRESENTATION_RELATIONSHIP_WITH_TRANSFORMATION(#60)
SHAPE_REPRESENTATION_RELATIONSHIP()
);
#166=(
REPRESENTATION_RELATIONSHIP($,$,#23867,#23826)
REPRESENTATION_RELATIONSHIP_WITH_TRANSFORMATION(#61)
SHAPE_REPRESENTATION_RELATIONSHIP()
);
#167=(
REPRESENTATION_RELATIONSHIP($,$,#23884,#23826)
REPRESENTATION_RELATIONSHIP_WITH_TRANSFORMATION(#62)
SHAPE_REPRESENTATION_RELATIONSHIP()
);
#168=(
REPRESENTATION_RELATIONSHIP($,$,#23884,#23826)
REPRESENTATION_RELATIONSHIP_WITH_TRANSFORMATION(#63)
SHAPE_REPRESENTATION_RELATIONSHIP()
);
#169=(
REPRESENTATION_RELATIONSHIP($,$,#23884,#23826)
REPRESENTATION_RELATIONSHIP_WITH_TRANSFORMATION(#64)
SHAPE_REPRESENTATION_RELATIONSHIP()
);
#170=(
REPRESENTATION_RELATIONSHIP($,$,#23884,#23826)
REPRESENTATION_RELATIONSHIP_WITH_TRANSFORMATION(#65)
SHAPE_REPRESENTATION_RELATIONSHIP()
);
#171=(
REPRESENTATION_RELATIONSHIP($,$,#23884,#23826)
REPRESENTATION_RELATIONSHIP_WITH_TRANSFORMATION(#66)
SHAPE_REPRESENTATION_RELATIONSHIP()
);
#172=(
REPRESENTATION_RELATIONSHIP($,$,#23884,#23826)
REPRESENTATION_RELATIONSHIP_WITH_TRANSFORMATION(#67)
SHAPE_REPRESENTATION_RELATIONSHIP()
);
#173=(
REPRESENTATION_RELATIONSHIP($,$,#23869,#23868)
REPRESENTATION_RELATIONSHIP_WITH_TRANSFORMATION(#68)
SHAPE_REPRESENTATION_RELATIONSHIP()
);
#174=(
REPRESENTATION_RELATIONSHIP($,$,#23870,#23868)
REPRESENTATION_RELATIONSHIP_WITH_TRANSFORMATION(#69)
SHAPE_REPRESENTATION_RELATIONSHIP()
);
#175=(
REPRESENTATION_RELATIONSHIP($,$,#23871,#23868)
REPRESENTATION_RELATIONSHIP_WITH_TRANSFORMATION(#70)
SHAPE_REPRESENTATION_RELATIONSHIP()
);
#176=(
REPRESENTATION_RELATIONSHIP($,$,#23872,#23868)
REPRESENTATION_RELATIONSHIP_WITH_TRANSFORMATION(#71)
SHAPE_REPRESENTATION_RELATIONSHIP()
);
#177=(
REPRESENTATION_RELATIONSHIP($,$,#23873,#23868)
REPRESENTATION_RELATIONSHIP_WITH_TRANSFORMATION(#72)
SHAPE_REPRESENTATION_RELATIONSHIP()
);
#178=(
REPRESENTATION_RELATIONSHIP($,$,#23874,#23868)
REPRESENTATION_RELATIONSHIP_WITH_TRANSFORMATION(#73)
SHAPE_REPRESENTATION_RELATIONSHIP()
);
#179=(
REPRESENTATION_RELATIONSHIP($,$,#23875,#23868)
REPRESENTATION_RELATIONSHIP_WITH_TRANSFORMATION(#74)
SHAPE_REPRESENTATION_RELATIONSHIP()
);
#180=(
REPRESENTATION_RELATIONSHIP($,$,#23884,#23868)
REPRESENTATION_RELATIONSHIP_WITH_TRANSFORMATION(#75)
SHAPE_REPRESENTATION_RELATIONSHIP()
);
#181=(
REPRESENTATION_RELATIONSHIP($,$,#23877,#23876)
REPRESENTATION_RELATIONSHIP_WITH_TRANSFORMATION(#76)
SHAPE_REPRESENTATION_RELATIONSHIP()
);
#182=(
REPRESENTATION_RELATIONSHIP($,$,#23878,#23876)
REPRESENTATION_RELATIONSHIP_WITH_TRANSFORMATION(#77)
SHAPE_REPRESENTATION_RELATIONSHIP()
);
#183=(
REPRESENTATION_RELATIONSHIP($,$,#23879,#23876)
REPRESENTATION_RELATIONSHIP_WITH_TRANSFORMATION(#78)
SHAPE_REPRESENTATION_RELATIONSHIP()
);
#184=(
REPRESENTATION_RELATIONSHIP($,$,#23880,#23876)
REPRESENTATION_RELATIONSHIP_WITH_TRANSFORMATION(#79)
SHAPE_REPRESENTATION_RELATIONSHIP()
);
#185=(
REPRESENTATION_RELATIONSHIP($,$,#23881,#23876)
REPRESENTATION_RELATIONSHIP_WITH_TRANSFORMATION(#80)
SHAPE_REPRESENTATION_RELATIONSHIP()
);
#186=(
REPRESENTATION_RELATIONSHIP($,$,#23882,#23876)
REPRESENTATION_RELATIONSHIP_WITH_TRANSFORMATION(#81)
SHAPE_REPRESENTATION_RELATIONSHIP()
);
#187=(
REPRESENTATION_RELATIONSHIP($,$,#23883,#23876)
REPRESENTATION_RELATIONSHIP_WITH_TRANSFORMATION(#82)
SHAPE_REPRESENTATION_RELATIONSHIP()
);
#188=(
REPRESENTATION_RELATIONSHIP($,$,#23884,#23876)
REPRESENTATION_RELATIONSHIP_WITH_TRANSFORMATION(#83)
SHAPE_REPRESENTATION_RELATIONSHIP()
);
#189=(
REPRESENTATION_RELATIONSHIP($,$,#23848,#23847)
REPRESENTATION_RELATIONSHIP_WITH_TRANSFORMATION(#84)
SHAPE_REPRESENTATION_RELATIONSHIP()
);
#190=(
REPRESENTATION_RELATIONSHIP($,$,#23849,#23847)
REPRESENTATION_RELATIONSHIP_WITH_TRANSFORMATION(#85)
SHAPE_REPRESENTATION_RELATIONSHIP()
);
#191=(
REPRESENTATION_RELATIONSHIP($,$,#23850,#23847)
REPRESENTATION_RELATIONSHIP_WITH_TRANSFORMATION(#86)
SHAPE_REPRESENTATION_RELATIONSHIP()
);
#192=(
REPRESENTATION_RELATIONSHIP($,$,#23851,#23847)
REPRESENTATION_RELATIONSHIP_WITH_TRANSFORMATION(#87)
SHAPE_REPRESENTATION_RELATIONSHIP()
);
#193=(
REPRESENTATION_RELATIONSHIP($,$,#23852,#23847)
REPRESENTATION_RELATIONSHIP_WITH_TRANSFORMATION(#88)
SHAPE_REPRESENTATION_RELATIONSHIP()
);
#194=(
REPRESENTATION_RELATIONSHIP($,$,#23853,#23847)
REPRESENTATION_RELATIONSHIP_WITH_TRANSFORMATION(#89)
SHAPE_REPRESENTATION_RELATIONSHIP()
);
#195=(
REPRESENTATION_RELATIONSHIP($,$,#23854,#23847)
REPRESENTATION_RELATIONSHIP_WITH_TRANSFORMATION(#90)
SHAPE_REPRESENTATION_RELATIONSHIP()
);
#196=(
REPRESENTATION_RELATIONSHIP($,$,#23855,#23847)
REPRESENTATION_RELATIONSHIP_WITH_TRANSFORMATION(#91)
SHAPE_REPRESENTATION_RELATIONSHIP()
);
#197=(
REPRESENTATION_RELATIONSHIP($,$,#23856,#23847)
REPRESENTATION_RELATIONSHIP_WITH_TRANSFORMATION(#92)
SHAPE_REPRESENTATION_RELATIONSHIP()
);
#198=(
REPRESENTATION_RELATIONSHIP($,$,#23860,#23847)
REPRESENTATION_RELATIONSHIP_WITH_TRANSFORMATION(#93)
SHAPE_REPRESENTATION_RELATIONSHIP()
);
#199=(
REPRESENTATION_RELATIONSHIP($,$,#23860,#23847)
REPRESENTATION_RELATIONSHIP_WITH_TRANSFORMATION(#94)
SHAPE_REPRESENTATION_RELATIONSHIP()
);
#200=(
REPRESENTATION_RELATIONSHIP($,$,#23860,#23847)
REPRESENTATION_RELATIONSHIP_WITH_TRANSFORMATION(#95)
SHAPE_REPRESENTATION_RELATIONSHIP()
);
#201=(
REPRESENTATION_RELATIONSHIP($,$,#23860,#23847)
REPRESENTATION_RELATIONSHIP_WITH_TRANSFORMATION(#96)
SHAPE_REPRESENTATION_RELATIONSHIP()
);
#202=(
REPRESENTATION_RELATIONSHIP($,$,#23884,#23847)
REPRESENTATION_RELATIONSHIP_WITH_TRANSFORMATION(#97)
SHAPE_REPRESENTATION_RELATIONSHIP()
);
#203=(
REPRESENTATION_RELATIONSHIP($,$,#23884,#23847)
REPRESENTATION_RELATIONSHIP_WITH_TRANSFORMATION(#98)
SHAPE_REPRESENTATION_RELATIONSHIP()
);
#204=(
REPRESENTATION_RELATIONSHIP($,$,#23884,#23847)
REPRESENTATION_RELATIONSHIP_WITH_TRANSFORMATION(#99)
SHAPE_REPRESENTATION_RELATIONSHIP()
);
#205=(
REPRESENTATION_RELATIONSHIP($,$,#23884,#23847)
REPRESENTATION_RELATIONSHIP_WITH_TRANSFORMATION(#100)
SHAPE_REPRESENTATION_RELATIONSHIP()
);
#206=(
REPRESENTATION_RELATIONSHIP($,$,#23861,#23847)
REPRESENTATION_RELATIONSHIP_WITH_TRANSFORMATION(#101)
SHAPE_REPRESENTATION_RELATIONSHIP()
);
#207=(
REPRESENTATION_RELATIONSHIP($,$,#23861,#23847)
REPRESENTATION_RELATIONSHIP_WITH_TRANSFORMATION(#102)
SHAPE_REPRESENTATION_RELATIONSHIP()
);
#208=(
REPRESENTATION_RELATIONSHIP($,$,#23867,#23847)
REPRESENTATION_RELATIONSHIP_WITH_TRANSFORMATION(#103)
SHAPE_REPRESENTATION_RELATIONSHIP()
);
#209=(
REPRESENTATION_RELATIONSHIP($,$,#23867,#23847)
REPRESENTATION_RELATIONSHIP_WITH_TRANSFORMATION(#104)
SHAPE_REPRESENTATION_RELATIONSHIP()
);
#210=(
REPRESENTATION_RELATIONSHIP($,$,#23867,#23847)
REPRESENTATION_RELATIONSHIP_WITH_TRANSFORMATION(#105)
SHAPE_REPRESENTATION_RELATIONSHIP()
);
#211=(
REPRESENTATION_RELATIONSHIP($,$,#23867,#23847)
REPRESENTATION_RELATIONSHIP_WITH_TRANSFORMATION(#106)
SHAPE_REPRESENTATION_RELATIONSHIP()
);
#212=(
REPRESENTATION_RELATIONSHIP($,$,#23867,#23847)
REPRESENTATION_RELATIONSHIP_WITH_TRANSFORMATION(#107)
SHAPE_REPRESENTATION_RELATIONSHIP()
);
#213=(
REPRESENTATION_RELATIONSHIP($,$,#23867,#23847)
REPRESENTATION_RELATIONSHIP_WITH_TRANSFORMATION(#108)
SHAPE_REPRESENTATION_RELATIONSHIP()
);
#214=(
REPRESENTATION_RELATIONSHIP($,$,#23867,#23847)
REPRESENTATION_RELATIONSHIP_WITH_TRANSFORMATION(#109)
SHAPE_REPRESENTATION_RELATIONSHIP()
);
#215=(
REPRESENTATION_RELATIONSHIP($,$,#23867,#23847)
REPRESENTATION_RELATIONSHIP_WITH_TRANSFORMATION(#110)
SHAPE_REPRESENTATION_RELATIONSHIP()
);
#216=(
REPRESENTATION_RELATIONSHIP($,$,#23884,#23847)
REPRESENTATION_RELATIONSHIP_WITH_TRANSFORMATION(#111)
SHAPE_REPRESENTATION_RELATIONSHIP()
);
#217=(
REPRESENTATION_RELATIONSHIP($,$,#23884,#23847)
REPRESENTATION_RELATIONSHIP_WITH_TRANSFORMATION(#112)
SHAPE_REPRESENTATION_RELATIONSHIP()
);
#218=(
REPRESENTATION_RELATIONSHIP($,$,#23888,#23847)
REPRESENTATION_RELATIONSHIP_WITH_TRANSFORMATION(#113)
SHAPE_REPRESENTATION_RELATIONSHIP()
);
#219=(
REPRESENTATION_RELATIONSHIP($,$,#23886,#23885)
REPRESENTATION_RELATIONSHIP_WITH_TRANSFORMATION(#114)
SHAPE_REPRESENTATION_RELATIONSHIP()
);
#220=(
REPRESENTATION_RELATIONSHIP($,$,#23887,#23885)
REPRESENTATION_RELATIONSHIP_WITH_TRANSFORMATION(#115)
SHAPE_REPRESENTATION_RELATIONSHIP()
);
#221=(
REPRESENTATION_RELATIONSHIP($,$,#23888,#23885)
REPRESENTATION_RELATIONSHIP_WITH_TRANSFORMATION(#116)
SHAPE_REPRESENTATION_RELATIONSHIP()
);
#222=(
REPRESENTATION_RELATIONSHIP($,$,#23826,#23825)
REPRESENTATION_RELATIONSHIP_WITH_TRANSFORMATION(#117)
SHAPE_REPRESENTATION_RELATIONSHIP()
);
#223=(
REPRESENTATION_RELATIONSHIP($,$,#23847,#23825)
REPRESENTATION_RELATIONSHIP_WITH_TRANSFORMATION(#118)
SHAPE_REPRESENTATION_RELATIONSHIP()
);
#224=(
REPRESENTATION_RELATIONSHIP($,$,#23868,#23825)
REPRESENTATION_RELATIONSHIP_WITH_TRANSFORMATION(#119)
SHAPE_REPRESENTATION_RELATIONSHIP()
);
#225=(
REPRESENTATION_RELATIONSHIP($,$,#23876,#23825)
REPRESENTATION_RELATIONSHIP_WITH_TRANSFORMATION(#120)
SHAPE_REPRESENTATION_RELATIONSHIP()
);
#226=(
REPRESENTATION_RELATIONSHIP($,$,#23885,#23825)
REPRESENTATION_RELATIONSHIP_WITH_TRANSFORMATION(#121)
SHAPE_REPRESENTATION_RELATIONSHIP()
);
#227=CONTEXT_DEPENDENT_SHAPE_REPRESENTATION(#122,#23678);
#228=CONTEXT_DEPENDENT_SHAPE_REPRESENTATION(#123,#23679);
#229=CONTEXT_DEPENDENT_SHAPE_REPRESENTATION(#124,#23680);
#230=CONTEXT_DEPENDENT_SHAPE_REPRESENTATION(#125,#23681);
#231=CONTEXT_DEPENDENT_SHAPE_REPRESENTATION(#126,#23682);
#232=CONTEXT_DEPENDENT_SHAPE_REPRESENTATION(#127,#23696);
#233=CONTEXT_DEPENDENT_SHAPE_REPRESENTATION(#128,#23697);
#234=CONTEXT_DEPENDENT_SHAPE_REPRESENTATION(#129,#23698);
#235=CONTEXT_DEPENDENT_SHAPE_REPRESENTATION(#130,#23706);
#236=CONTEXT_DEPENDENT_SHAPE_REPRESENTATION(#131,#23707);
#237=CONTEXT_DEPENDENT_SHAPE_REPRESENTATION(#132,#23708);
#238=CONTEXT_DEPENDENT_SHAPE_REPRESENTATION(#133,#23709);
#239=CONTEXT_DEPENDENT_SHAPE_REPRESENTATION(#134,#23710);
#240=CONTEXT_DEPENDENT_SHAPE_REPRESENTATION(#135,#23729);
#241=CONTEXT_DEPENDENT_SHAPE_REPRESENTATION(#136,#23730);
#242=CONTEXT_DEPENDENT_SHAPE_REPRESENTATION(#137,#23731);
#243=CONTEXT_DEPENDENT_SHAPE_REPRESENTATION(#138,#23732);
#244=CONTEXT_DEPENDENT_SHAPE_REPRESENTATION(#139,#23733);
#245=CONTEXT_DEPENDENT_SHAPE_REPRESENTATION(#140,#23734);
#246=CONTEXT_DEPENDENT_SHAPE_REPRESENTATION(#141,#23735);
#247=CONTEXT_DEPENDENT_SHAPE_REPRESENTATION(#142,#23736);
#248=CONTEXT_DEPENDENT_SHAPE_REPRESENTATION(#143,#23737);
#249=CONTEXT_DEPENDENT_SHAPE_REPRESENTATION(#144,#23738);
#250=CONTEXT_DEPENDENT_SHAPE_REPRESENTATION(#145,#23739);
#251=CONTEXT_DEPENDENT_SHAPE_REPRESENTATION(#146,#23740);
#252=CONTEXT_DEPENDENT_SHAPE_REPRESENTATION(#147,#23741);
#253=CONTEXT_DEPENDENT_SHAPE_REPRESENTATION(#148,#23742);
#254=CONTEXT_DEPENDENT_SHAPE_REPRESENTATION(#149,#23743);
#255=CONTEXT_DEPENDENT_SHAPE_REPRESENTATION(#150,#23744);
#256=CONTEXT_DEPENDENT_SHAPE_REPRESENTATION(#151,#23745);
#257=CONTEXT_DEPENDENT_SHAPE_REPRESENTATION(#152,#23746);
#258=CONTEXT_DEPENDENT_SHAPE_REPRESENTATION(#153,#23747);
#259=CONTEXT_DEPENDENT_SHAPE_REPRESENTATION(#154,#23748);
#260=CONTEXT_DEPENDENT_SHAPE_REPRESENTATION(#155,#23749);
#261=CONTEXT_DEPENDENT_SHAPE_REPRESENTATION(#156,#23750);
#262=CONTEXT_DEPENDENT_SHAPE_REPRESENTATION(#157,#23751);
#263=CONTEXT_DEPENDENT_SHAPE_REPRESENTATION(#158,#23752);
#264=CONTEXT_DEPENDENT_SHAPE_REPRESENTATION(#159,#23753);
#265=CONTEXT_DEPENDENT_SHAPE_REPRESENTATION(#160,#23754);
#266=CONTEXT_DEPENDENT_SHAPE_REPRESENTATION(#161,#23755);
#267=CONTEXT_DEPENDENT_SHAPE_REPRESENTATION(#162,#23756);
#268=CONTEXT_DEPENDENT_SHAPE_REPRESENTATION(#163,#23757);
#269=CONTEXT_DEPENDENT_SHAPE_REPRESENTATION(#164,#23758);
#270=CONTEXT_DEPENDENT_SHAPE_REPRESENTATION(#165,#23759);
#271=CONTEXT_DEPENDENT_SHAPE_REPRESENTATION(#166,#23760);
#272=CONTEXT_DEPENDENT_SHAPE_REPRESENTATION(#167,#23761);
#273=CONTEXT_DEPENDENT_SHAPE_REPRESENTATION(#168,#23762);
#274=CONTEXT_DEPENDENT_SHAPE_REPRESENTATION(#169,#23763);
#275=CONTEXT_DEPENDENT_SHAPE_REPRESENTATION(#170,#23764);
#276=CONTEXT_DEPENDENT_SHAPE_REPRESENTATION(#171,#23765);
#277=CONTEXT_DEPENDENT_SHAPE_REPRESENTATION(#172,#23766);
#278=CONTEXT_DEPENDENT_SHAPE_REPRESENTATION(#173,#23767);
#279=CONTEXT_DEPENDENT_SHAPE_REPRESENTATION(#174,#23768);
#280=CONTEXT_DEPENDENT_SHAPE_REPRESENTATION(#175,#23769);
#281=CONTEXT_DEPENDENT_SHAPE_REPRESENTATION(#176,#23770);
#282=CONTEXT_DEPENDENT_SHAPE_REPRESENTATION(#177,#23771);
#283=CONTEXT_DEPENDENT_SHAPE_REPRESENTATION(#178,#23772);
#284=CONTEXT_DEPENDENT_SHAPE_REPRESENTATION(#179,#23773);
#285=CONTEXT_DEPENDENT_SHAPE_REPRESENTATION(#180,#23774);
#286=CONTEXT_DEPENDENT_SHAPE_REPRESENTATION(#181,#23775);
#287=CONTEXT_DEPENDENT_SHAPE_REPRESENTATION(#182,#23776);
#288=CONTEXT_DEPENDENT_SHAPE_REPRESENTATION(#183,#23777);
#289=CONTEXT_DEPENDENT_SHAPE_REPRESENTATION(#184,#23778);
#290=CONTEXT_DEPENDENT_SHAPE_REPRESENTATION(#185,#23779);
#291=CONTEXT_DEPENDENT_SHAPE_REPRESENTATION(#186,#23780);
#292=CONTEXT_DEPENDENT_SHAPE_REPRESENTATION(#187,#23781);
#293=CONTEXT_DEPENDENT_SHAPE_REPRESENTATION(#188,#23782);
#294=CONTEXT_DEPENDENT_SHAPE_REPRESENTATION(#189,#23787);
#295=CONTEXT_DEPENDENT_SHAPE_REPRESENTATION(#190,#23788);
#296=CONTEXT_DEPENDENT_SHAPE_REPRESENTATION(#191,#23789);
#297=CONTEXT_DEPENDENT_SHAPE_REPRESENTATION(#192,#23790);
#298=CONTEXT_DEPENDENT_SHAPE_REPRESENTATION(#193,#23791);
#299=CONTEXT_DEPENDENT_SHAPE_REPRESENTATION(#194,#23792);
#300=CONTEXT_DEPENDENT_SHAPE_REPRESENTATION(#195,#23793);
#301=CONTEXT_DEPENDENT_SHAPE_REPRESENTATION(#196,#23794);
#302=CONTEXT_DEPENDENT_SHAPE_REPRESENTATION(#197,#23795);
#303=CONTEXT_DEPENDENT_SHAPE_REPRESENTATION(#198,#23796);
#304=CONTEXT_DEPENDENT_SHAPE_REPRESENTATION(#199,#23797);
#305=CONTEXT_DEPENDENT_SHAPE_REPRESENTATION(#200,#23798);
#306=CONTEXT_DEPENDENT_SHAPE_REPRESENTATION(#201,#23799);
#307=CONTEXT_DEPENDENT_SHAPE_REPRESENTATION(#202,#23800);
#308=CONTEXT_DEPENDENT_SHAPE_REPRESENTATION(#203,#23801);
#309=CONTEXT_DEPENDENT_SHAPE_REPRESENTATION(#204,#23802);
#310=CONTEXT_DEPENDENT_SHAPE_REPRESENTATION(#205,#23803);
#311=CONTEXT_DEPENDENT_SHAPE_REPRESENTATION(#206,#23804);
#312=CONTEXT_DEPENDENT_SHAPE_REPRESENTATION(#207,#23805);
#313=CONTEXT_DEPENDENT_SHAPE_REPRESENTATION(#208,#23806);
#314=CONTEXT_DEPENDENT_SHAPE_REPRESENTATION(#209,#23807);
#315=CONTEXT_DEPENDENT_SHAPE_REPRESENTATION(#210,#23808);
#316=CONTEXT_DEPENDENT_SHAPE_REPRESENTATION(#211,#23809);
#317=CONTEXT_DEPENDENT_SHAPE_REPRESENTATION(#212,#23810);
#318=CONTEXT_DEPENDENT_SHAPE_REPRESENTATION(#213,#23811);
#319=CONTEXT_DEPENDENT_SHAPE_REPRESENTATION(#214,#23812);
#320=CONTEXT_DEPENDENT_SHAPE_REPRESENTATION(#215,#23813);
#321=CONTEXT_DEPENDENT_SHAPE_REPRESENTATION(#216,#23814);
#322=CONTEXT_DEPENDENT_SHAPE_REPRESENTATION(#217,#23815);
#323=CONTEXT_DEPENDENT_SHAPE_REPRESENTATION(#218,#23816);
#324=CONTEXT_DEPENDENT_SHAPE_REPRESENTATION(#219,#23817);
#325=CONTEXT_DEPENDENT_SHAPE_REPRESENTATION(#220,#23818);
#326=CONTEXT_DEPENDENT_SHAPE_REPRESENTATION(#221,#23819);
#327=CONTEXT_DEPENDENT_SHAPE_REPRESENTATION(#222,#23820);
#328=CONTEXT_DEPENDENT_SHAPE_REPRESENTATION(#223,#23821);
#329=CONTEXT_DEPENDENT_SHAPE_REPRESENTATION(#224,#23822);
#330=CONTEXT_DEPENDENT_SHAPE_REPRESENTATION(#225,#23823);
#331=CONTEXT_DEPENDENT_SHAPE_REPRESENTATION(#226,#23824);
#332=NEXT_ASSEMBLY_USAGE_OCCURRENCE('Inner ring:1','Inner ring:1',
'Inner ring:1',#23906,#23907,'Inner ring:1');
#333=NEXT_ASSEMBLY_USAGE_OCCURRENCE('Outer ring:1','Outer ring:1',
'Outer ring:1',#23906,#23908,'Outer ring:1');
#334=NEXT_ASSEMBLY_USAGE_OCCURRENCE('Balls:1','Balls:1','Balls:1',#23906,
#23909,'Balls:1');
#335=NEXT_ASSEMBLY_USAGE_OCCURRENCE('Cage:1','Cage:1','Cage:1',#23906,#23910,
'Cage:1');
#336=NEXT_ASSEMBLY_USAGE_OCCURRENCE('Seals 2RS:1','Seals 2RS:1',
'Seals 2RS:1',#23906,#23911,'Seals 2RS:1');
#337=NEXT_ASSEMBLY_USAGE_OCCURRENCE('Block:1','Block:1','Block:1',#23921,
#23922,'Block:1');
#338=NEXT_ASSEMBLY_USAGE_OCCURRENCE('End cap +:1','End cap +:1',
'End cap +:1',#23921,#23923,'End cap +:1');
#339=NEXT_ASSEMBLY_USAGE_OCCURRENCE('End cap:1','End cap:1','End cap:1',
#23921,#23924,'End cap:1');
#340=NEXT_ASSEMBLY_USAGE_OCCURRENCE('Inner ring (1):1',
'Inner ring (1):1','Inner ring (1):1',#23926,#23927,'Inner ring (1):1');
#341=NEXT_ASSEMBLY_USAGE_OCCURRENCE('Outer ring (1):1',
'Outer ring (1):1','Outer ring (1):1',#23926,#23928,'Outer ring (1):1');
#342=NEXT_ASSEMBLY_USAGE_OCCURRENCE('Balls (1):1','Balls (1):1',
'Balls (1):1',#23926,#23929,'Balls (1):1');
#343=NEXT_ASSEMBLY_USAGE_OCCURRENCE('Cage (1):1','Cage (1):1',
'Cage (1):1',#23926,#23930,'Cage (1):1');
#344=NEXT_ASSEMBLY_USAGE_OCCURRENCE('Seals 2RS (1):1','Seals 2RS (1):1',
'Seals 2RS (1):1',#23926,#23931,'Seals 2RS (1):1');
#345=NEXT_ASSEMBLY_USAGE_OCCURRENCE('Base:1','Base:1','Base:1',#23891,#23892,
'Base:1');
#346=NEXT_ASSEMBLY_USAGE_OCCURRENCE('Foot:1','Foot:1','Foot:1',#23891,#23893,
'Foot:1');
#347=NEXT_ASSEMBLY_USAGE_OCCURRENCE('Foot (1):1','Foot (1):1',
'Foot (1):1',#23891,#23894,'Foot (1):1');
#348=NEXT_ASSEMBLY_USAGE_OCCURRENCE('Fixed bearing block:1',
'Fixed bearing block:1','Fixed bearing block:1',#23891,#23895,
'Fixed bearing block:1');
#349=NEXT_ASSEMBLY_USAGE_OCCURRENCE('Input outer spacer:1',
'Input outer spacer:1','Input outer spacer:1',#23891,#23896,
'Input outer spacer:1');
#350=NEXT_ASSEMBLY_USAGE_OCCURRENCE('Input bearing cap:1',
'Input bearing cap:1','Input bearing cap:1',#23891,#23897,
'Input bearing cap:1');
#351=NEXT_ASSEMBLY_USAGE_OCCURRENCE('Input bearing cap (1):1',
'Input bearing cap (1):1','Input bearing cap (1):1',#23891,#23898,
'Input bearing cap (1):1');
#352=NEXT_ASSEMBLY_USAGE_OCCURRENCE('Screw support:1','Screw support:1',
'Screw support:1',#23891,#23899,'Screw support:1');
#353=NEXT_ASSEMBLY_USAGE_OCCURRENCE('Screw bushing:1','Screw bushing:1',
'Screw bushing:1',#23891,#23900,'Screw bushing:1');
#354=NEXT_ASSEMBLY_USAGE_OCCURRENCE('Screw support (1):1',
'Screw support (1):1','Screw support (1):1',#23891,#23901,
'Screw support (1):1');
#355=NEXT_ASSEMBLY_USAGE_OCCURRENCE('Screw bushing (1):1',
'Screw bushing (1):1','Screw bushing (1):1',#23891,#23902,
'Screw bushing (1):1');
#356=NEXT_ASSEMBLY_USAGE_OCCURRENCE('Force gauge envelope:1',
'Force gauge envelope:1','Force gauge envelope:1',#23891,#23903,
'Force gauge envelope:1');
#357=NEXT_ASSEMBLY_USAGE_OCCURRENCE('Gauge mounting saddle:1',
'Gauge mounting saddle:1','Gauge mounting saddle:1',#23891,#23904,
'Gauge mounting saddle:1');
#358=NEXT_ASSEMBLY_USAGE_OCCURRENCE(
'Linear Guide Rail - 15 mm, 220 mm Long:2',
'Linear Guide Rail - 15 mm, 220 mm Long:2',
'Linear Guide Rail - 15 mm, 220 mm Long:2',#23891,#23905,
'Linear Guide Rail - 15 mm, 220 mm Long:2');
#359=NEXT_ASSEMBLY_USAGE_OCCURRENCE('Cap Screw - M4x16:2',
'Cap Screw - M4x16:2','Cap Screw - M4x16:2',#23891,#23949,
'Cap Screw - M4x16:2');
#360=NEXT_ASSEMBLY_USAGE_OCCURRENCE('Cap Screw - M4x16:3',
'Cap Screw - M4x16:3','Cap Screw - M4x16:3',#23891,#23949,
'Cap Screw - M4x16:3');
#361=NEXT_ASSEMBLY_USAGE_OCCURRENCE('Cap Screw - M4x16:4',
'Cap Screw - M4x16:4','Cap Screw - M4x16:4',#23891,#23949,
'Cap Screw - M4x16:4');
#362=NEXT_ASSEMBLY_USAGE_OCCURRENCE('Cap Screw - M4x16:5',
'Cap Screw - M4x16:5','Cap Screw - M4x16:5',#23891,#23949,
'Cap Screw - M4x16:5');
#363=NEXT_ASSEMBLY_USAGE_OCCURRENCE('Cap Screw - M4x16:6',
'Cap Screw - M4x16:6','Cap Screw - M4x16:6',#23891,#23949,
'Cap Screw - M4x16:6');
#364=NEXT_ASSEMBLY_USAGE_OCCURRENCE('Cap Screw - M4x16:7',
'Cap Screw - M4x16:7','Cap Screw - M4x16:7',#23891,#23949,
'Cap Screw - M4x16:7');
#365=NEXT_ASSEMBLY_USAGE_OCCURRENCE('Cap Screw - M4x16:8',
'Cap Screw - M4x16:8','Cap Screw - M4x16:8',#23891,#23949,
'Cap Screw - M4x16:8');
#366=NEXT_ASSEMBLY_USAGE_OCCURRENCE('Cap Screw - M4x16:9',
'Cap Screw - M4x16:9','Cap Screw - M4x16:9',#23891,#23949,
'Cap Screw - M4x16:9');
#367=NEXT_ASSEMBLY_USAGE_OCCURRENCE(
'Sealed Ball Bearing - 10 x 30 x 9 mm:2',
'Sealed Ball Bearing - 10 x 30 x 9 mm:2',
'Sealed Ball Bearing - 10 x 30 x 9 mm:2',#23891,#23906,
'Sealed Ball Bearing - 10 x 30 x 9 mm:2');
#368=NEXT_ASSEMBLY_USAGE_OCCURRENCE(
'Sealed Ball Bearing - 10 x 30 x 9 mm:3',
'Sealed Ball Bearing - 10 x 30 x 9 mm:3',
'Sealed Ball Bearing - 10 x 30 x 9 mm:3',#23891,#23906,
'Sealed Ball Bearing - 10 x 30 x 9 mm:3');
#369=NEXT_ASSEMBLY_USAGE_OCCURRENCE('M4x10 Cap Screw:2',
'M4x10 Cap Screw:2','M4x10 Cap Screw:2',#23891,#23932,
'M4x10 Cap Screw:2');
#370=NEXT_ASSEMBLY_USAGE_OCCURRENCE('M4x10 Cap Screw:3',
'M4x10 Cap Screw:3','M4x10 Cap Screw:3',#23891,#23932,
'M4x10 Cap Screw:3');
#371=NEXT_ASSEMBLY_USAGE_OCCURRENCE('M4x10 Cap Screw:4',
'M4x10 Cap Screw:4','M4x10 Cap Screw:4',#23891,#23932,
'M4x10 Cap Screw:4');
#372=NEXT_ASSEMBLY_USAGE_OCCURRENCE('M4x10 Cap Screw:5',
'M4x10 Cap Screw:5','M4x10 Cap Screw:5',#23891,#23932,
'M4x10 Cap Screw:5');
#373=NEXT_ASSEMBLY_USAGE_OCCURRENCE('M4x10 Cap Screw:6',
'M4x10 Cap Screw:6','M4x10 Cap Screw:6',#23891,#23932,
'M4x10 Cap Screw:6');
#374=NEXT_ASSEMBLY_USAGE_OCCURRENCE('M4x10 Cap Screw:7',
'M4x10 Cap Screw:7','M4x10 Cap Screw:7',#23891,#23932,
'M4x10 Cap Screw:7');
#375=NEXT_ASSEMBLY_USAGE_OCCURRENCE('M4x10 Cap Screw:8',
'M4x10 Cap Screw:8','M4x10 Cap Screw:8',#23891,#23932,
'M4x10 Cap Screw:8');
#376=NEXT_ASSEMBLY_USAGE_OCCURRENCE('M4x10 Cap Screw:9',
'M4x10 Cap Screw:9','M4x10 Cap Screw:9',#23891,#23932,
'M4x10 Cap Screw:9');
#377=NEXT_ASSEMBLY_USAGE_OCCURRENCE('Cap Screw - M4x16:16',
'Cap Screw - M4x16:16','Cap Screw - M4x16:16',#23891,#23949,
'Cap Screw - M4x16:16');
#378=NEXT_ASSEMBLY_USAGE_OCCURRENCE('Cap Screw - M4x16:17',
'Cap Screw - M4x16:17','Cap Screw - M4x16:17',#23891,#23949,
'Cap Screw - M4x16:17');
#379=NEXT_ASSEMBLY_USAGE_OCCURRENCE('Cap Screw - M4x16:18',
'Cap Screw - M4x16:18','Cap Screw - M4x16:18',#23891,#23949,
'Cap Screw - M4x16:18');
#380=NEXT_ASSEMBLY_USAGE_OCCURRENCE('Cap Screw - M4x16:19',
'Cap Screw - M4x16:19','Cap Screw - M4x16:19',#23891,#23949,
'Cap Screw - M4x16:19');
#381=NEXT_ASSEMBLY_USAGE_OCCURRENCE('Cap Screw - M4x16:22',
'Cap Screw - M4x16:22','Cap Screw - M4x16:22',#23891,#23949,
'Cap Screw - M4x16:22');
#382=NEXT_ASSEMBLY_USAGE_OCCURRENCE('Cap Screw - M4x16:23',
'Cap Screw - M4x16:23','Cap Screw - M4x16:23',#23891,#23949,
'Cap Screw - M4x16:23');
#383=NEXT_ASSEMBLY_USAGE_OCCURRENCE('Input shaft:1','Input shaft:1',
'Input shaft:1',#23933,#23934,'Input shaft:1');
#384=NEXT_ASSEMBLY_USAGE_OCCURRENCE('Input inner spacer:1',
'Input inner spacer:1','Input inner spacer:1',#23933,#23935,
'Input inner spacer:1');
#385=NEXT_ASSEMBLY_USAGE_OCCURRENCE('Input inner sleeve:1',
'Input inner sleeve:1','Input inner sleeve:1',#23933,#23936,
'Input inner sleeve:1');
#386=NEXT_ASSEMBLY_USAGE_OCCURRENCE('Input M3 set screw:1',
'Input M3 set screw:1','Input M3 set screw:1',#23933,#23937,
'Input M3 set screw:1');
#387=NEXT_ASSEMBLY_USAGE_OCCURRENCE('Input M3 set screw (1):1',
'Input M3 set screw (1):1','Input M3 set screw (1):1',#23933,#23938,
'Input M3 set screw (1):1');
#388=NEXT_ASSEMBLY_USAGE_OCCURRENCE('Input end keeper:1',
'Input end keeper:1','Input end keeper:1',#23933,#23939,
'Input end keeper:1');
#389=NEXT_ASSEMBLY_USAGE_OCCURRENCE(
'Timing Pulley - 2 mm Pitch, 20 Teeth, 8 mm Bore:2',
'Timing Pulley - 2 mm Pitch, 20 Teeth, 8 mm Bore:2',
'Timing Pulley - 2 mm Pitch, 20 Teeth, 8 mm Bore:2',#23933,#23940,
'Timing Pulley - 2 mm Pitch, 20 Teeth, 8 mm Bore:2');
#390=NEXT_ASSEMBLY_USAGE_OCCURRENCE('Cap Screw - M4x16:10',
'Cap Screw - M4x16:10','Cap Screw - M4x16:10',#23933,#23949,
'Cap Screw - M4x16:10');
#391=NEXT_ASSEMBLY_USAGE_OCCURRENCE('Output shaft:1','Output shaft:1',
'Output shaft:1',#23941,#23942,'Output shaft:1');
#392=NEXT_ASSEMBLY_USAGE_OCCURRENCE('Output inner spacer:1',
'Output inner spacer:1','Output inner spacer:1',#23941,#23943,
'Output inner spacer:1');
#393=NEXT_ASSEMBLY_USAGE_OCCURRENCE('Output inner sleeve:1',
'Output inner sleeve:1','Output inner sleeve:1',#23941,#23944,
'Output inner sleeve:1');
#394=NEXT_ASSEMBLY_USAGE_OCCURRENCE('Output M3 set screw:1',
'Output M3 set screw:1','Output M3 set screw:1',#23941,#23945,
'Output M3 set screw:1');
#395=NEXT_ASSEMBLY_USAGE_OCCURRENCE('Output M3 set screw (1):1',
'Output M3 set screw (1):1','Output M3 set screw (1):1',#23941,#23946,
'Output M3 set screw (1):1');
#396=NEXT_ASSEMBLY_USAGE_OCCURRENCE('Output end keeper:1',
'Output end keeper:1','Output end keeper:1',#23941,#23947,
'Output end keeper:1');
#397=NEXT_ASSEMBLY_USAGE_OCCURRENCE(
'Timing Pulley - 2 mm Pitch, 40 Teeth, 12 mm Bore:2',
'Timing Pulley - 2 mm Pitch, 40 Teeth, 12 mm Bore:2',
'Timing Pulley - 2 mm Pitch, 40 Teeth, 12 mm Bore:2',#23941,#23948,
'Timing Pulley - 2 mm Pitch, 40 Teeth, 12 mm Bore:2');
#398=NEXT_ASSEMBLY_USAGE_OCCURRENCE('Cap Screw - M4x16:15',
'Cap Screw - M4x16:15','Cap Screw - M4x16:15',#23941,#23949,
'Cap Screw - M4x16:15');
#399=NEXT_ASSEMBLY_USAGE_OCCURRENCE('Sliding plate:1','Sliding plate:1',
'Sliding plate:1',#23912,#23913,'Sliding plate:1');
#400=NEXT_ASSEMBLY_USAGE_OCCURRENCE('Sliding bearing block:1',
'Sliding bearing block:1','Sliding bearing block:1',#23912,#23914,
'Sliding bearing block:1');
#401=NEXT_ASSEMBLY_USAGE_OCCURRENCE('Output outer spacer:1',
'Output outer spacer:1','Output outer spacer:1',#23912,#23915,
'Output outer spacer:1');
#402=NEXT_ASSEMBLY_USAGE_OCCURRENCE('Output bearing cap:1',
'Output bearing cap:1','Output bearing cap:1',#23912,#23916,
'Output bearing cap:1');
#403=NEXT_ASSEMBLY_USAGE_OCCURRENCE('Output bearing cap (1):1',
'Output bearing cap (1):1','Output bearing cap (1):1',#23912,#23917,
'Output bearing cap (1):1');
#404=NEXT_ASSEMBLY_USAGE_OCCURRENCE('Adjusting nut pedestal:1',
'Adjusting nut pedestal:1','Adjusting nut pedestal:1',#23912,#23918,
'Adjusting nut pedestal:1');
#405=NEXT_ASSEMBLY_USAGE_OCCURRENCE('Gauge extension rod:1',
'Gauge extension rod:1','Gauge extension rod:1',#23912,#23919,
'Gauge extension rod:1');
#406=NEXT_ASSEMBLY_USAGE_OCCURRENCE('Gauge rod bracket:1',
'Gauge rod bracket:1','Gauge rod bracket:1',#23912,#23920,
'Gauge rod bracket:1');
#407=NEXT_ASSEMBLY_USAGE_OCCURRENCE(
'Flanged Linear Guide Carriage - 15 mm:2',
'Flanged Linear Guide Carriage - 15 mm:2',
'Flanged Linear Guide Carriage - 15 mm:2',#23912,#23921,
'Flanged Linear Guide Carriage - 15 mm:2');
#408=NEXT_ASSEMBLY_USAGE_OCCURRENCE('M5x14 Cap Screw:2',
'M5x14 Cap Screw:2','M5x14 Cap Screw:2',#23912,#23925,
'M5x14 Cap Screw:2');
#409=NEXT_ASSEMBLY_USAGE_OCCURRENCE('M5x14 Cap Screw:3',
'M5x14 Cap Screw:3','M5x14 Cap Screw:3',#23912,#23925,
'M5x14 Cap Screw:3');
#410=NEXT_ASSEMBLY_USAGE_OCCURRENCE('M5x14 Cap Screw:4',
'M5x14 Cap Screw:4','M5x14 Cap Screw:4',#23912,#23925,
'M5x14 Cap Screw:4');
#411=NEXT_ASSEMBLY_USAGE_OCCURRENCE('M5x14 Cap Screw:5',
'M5x14 Cap Screw:5','M5x14 Cap Screw:5',#23912,#23925,
'M5x14 Cap Screw:5');
#412=NEXT_ASSEMBLY_USAGE_OCCURRENCE('Cap Screw - M4x16:11',
'Cap Screw - M4x16:11','Cap Screw - M4x16:11',#23912,#23949,
'Cap Screw - M4x16:11');
#413=NEXT_ASSEMBLY_USAGE_OCCURRENCE('Cap Screw - M4x16:12',
'Cap Screw - M4x16:12','Cap Screw - M4x16:12',#23912,#23949,
'Cap Screw - M4x16:12');
#414=NEXT_ASSEMBLY_USAGE_OCCURRENCE('Cap Screw - M4x16:13',
'Cap Screw - M4x16:13','Cap Screw - M4x16:13',#23912,#23949,
'Cap Screw - M4x16:13');
#415=NEXT_ASSEMBLY_USAGE_OCCURRENCE('Cap Screw - M4x16:14',
'Cap Screw - M4x16:14','Cap Screw - M4x16:14',#23912,#23949,
'Cap Screw - M4x16:14');
#416=NEXT_ASSEMBLY_USAGE_OCCURRENCE(
'Sealed Ball Bearing - 12 x 32 x 10 mm:2',
'Sealed Ball Bearing - 12 x 32 x 10 mm:2',
'Sealed Ball Bearing - 12 x 32 x 10 mm:2',#23912,#23926,
'Sealed Ball Bearing - 12 x 32 x 10 mm:2');
#417=NEXT_ASSEMBLY_USAGE_OCCURRENCE(
'Sealed Ball Bearing - 12 x 32 x 10 mm:3',
'Sealed Ball Bearing - 12 x 32 x 10 mm:3',
'Sealed Ball Bearing - 12 x 32 x 10 mm:3',#23912,#23926,
'Sealed Ball Bearing - 12 x 32 x 10 mm:3');
#418=NEXT_ASSEMBLY_USAGE_OCCURRENCE('M4x10 Cap Screw:10',
'M4x10 Cap Screw:10','M4x10 Cap Screw:10',#23912,#23932,
'M4x10 Cap Screw:10');
#419=NEXT_ASSEMBLY_USAGE_OCCURRENCE('M4x10 Cap Screw:11',
'M4x10 Cap Screw:11','M4x10 Cap Screw:11',#23912,#23932,
'M4x10 Cap Screw:11');
#420=NEXT_ASSEMBLY_USAGE_OCCURRENCE('M4x10 Cap Screw:12',
'M4x10 Cap Screw:12','M4x10 Cap Screw:12',#23912,#23932,
'M4x10 Cap Screw:12');
#421=NEXT_ASSEMBLY_USAGE_OCCURRENCE('M4x10 Cap Screw:13',
'M4x10 Cap Screw:13','M4x10 Cap Screw:13',#23912,#23932,
'M4x10 Cap Screw:13');
#422=NEXT_ASSEMBLY_USAGE_OCCURRENCE('M4x10 Cap Screw:14',
'M4x10 Cap Screw:14','M4x10 Cap Screw:14',#23912,#23932,
'M4x10 Cap Screw:14');
#423=NEXT_ASSEMBLY_USAGE_OCCURRENCE('M4x10 Cap Screw:15',
'M4x10 Cap Screw:15','M4x10 Cap Screw:15',#23912,#23932,
'M4x10 Cap Screw:15');
#424=NEXT_ASSEMBLY_USAGE_OCCURRENCE('M4x10 Cap Screw:16',
'M4x10 Cap Screw:16','M4x10 Cap Screw:16',#23912,#23932,
'M4x10 Cap Screw:16');
#425=NEXT_ASSEMBLY_USAGE_OCCURRENCE('M4x10 Cap Screw:17',
'M4x10 Cap Screw:17','M4x10 Cap Screw:17',#23912,#23932,
'M4x10 Cap Screw:17');
#426=NEXT_ASSEMBLY_USAGE_OCCURRENCE('Cap Screw - M4x16:20',
'Cap Screw - M4x16:20','Cap Screw - M4x16:20',#23912,#23949,
'Cap Screw - M4x16:20');
#427=NEXT_ASSEMBLY_USAGE_OCCURRENCE('Cap Screw - M4x16:21',
'Cap Screw - M4x16:21','Cap Screw - M4x16:21',#23912,#23949,
'Cap Screw - M4x16:21');
#428=NEXT_ASSEMBLY_USAGE_OCCURRENCE('Socket Set Screw - M4x6:3',
'Socket Set Screw - M4x6:3','Socket Set Screw - M4x6:3',#23912,#23953,
'Socket Set Screw - M4x6:3');
#429=NEXT_ASSEMBLY_USAGE_OCCURRENCE('M8x1.25 adjusting spindle:1',
'M8x1.25 adjusting spindle:1','M8x1.25 adjusting spindle:1',#23950,#23951,
'M8x1.25 adjusting spindle:1');
#430=NEXT_ASSEMBLY_USAGE_OCCURRENCE('Adjusting knob:1',
'Adjusting knob:1','Adjusting knob:1',#23950,#23952,'Adjusting knob:1');
#431=NEXT_ASSEMBLY_USAGE_OCCURRENCE('Socket Set Screw - M4x6:2',
'Socket Set Screw - M4x6:2','Socket Set Screw - M4x6:2',#23950,#23953,
'Socket Set Screw - M4x6:2');
#432=NEXT_ASSEMBLY_USAGE_OCCURRENCE('Base and guide:1',
'Base and guide:1','Base and guide:1',#23890,#23891,'Base and guide:1');
#433=NEXT_ASSEMBLY_USAGE_OCCURRENCE('Sliding bearing and gauge rod:1',
'Sliding bearing and gauge rod:1','Sliding bearing and gauge rod:1',#23890,
#23912,'Sliding bearing and gauge rod:1');
#434=NEXT_ASSEMBLY_USAGE_OCCURRENCE('Input pulley:1','Input pulley:1',
'Input pulley:1',#23890,#23933,'Input pulley:1');
#435=NEXT_ASSEMBLY_USAGE_OCCURRENCE('Sliding pulley:1',
'Sliding pulley:1','Sliding pulley:1',#23890,#23941,'Sliding pulley:1');
#436=NEXT_ASSEMBLY_USAGE_OCCURRENCE('Adjusting screw:1',
'Adjusting screw:1','Adjusting screw:1',#23890,#23950,
'Adjusting screw:1');
#437=SPHERICAL_SURFACE('',#13263,0.23815);
#438=SPHERICAL_SURFACE('',#13265,0.23815);
#439=SPHERICAL_SURFACE('',#13267,0.23815);
#440=SPHERICAL_SURFACE('',#13269,0.23815);
#441=SPHERICAL_SURFACE('',#13271,0.23815);
#442=SPHERICAL_SURFACE('',#13273,0.23815);
#443=SPHERICAL_SURFACE('',#13275,0.23815);
#444=SPHERICAL_SURFACE('',#13277,0.23815);
#445=SPHERICAL_SURFACE('',#13280,0.247676);
#446=SPHERICAL_SURFACE('',#13296,0.247676);
#447=SPHERICAL_SURFACE('',#13301,0.247676);
#448=SPHERICAL_SURFACE('',#13306,0.247676);
#449=SPHERICAL_SURFACE('',#13311,0.247676);
#450=SPHERICAL_SURFACE('',#13316,0.247676);
#451=SPHERICAL_SURFACE('',#13321,0.247676);
#452=SPHERICAL_SURFACE('',#13329,0.247676);
#453=SPHERICAL_SURFACE('',#13695,0.29765);
#454=SPHERICAL_SURFACE('',#13697,0.29765);
#455=SPHERICAL_SURFACE('',#13699,0.29765);
#456=SPHERICAL_SURFACE('',#13701,0.29765);
#457=SPHERICAL_SURFACE('',#13703,0.29765);
#458=SPHERICAL_SURFACE('',#13705,0.29765);
#459=SPHERICAL_SURFACE('',#13707,0.29765);
#460=SPHERICAL_SURFACE('',#13710,0.309556);
#461=SPHERICAL_SURFACE('',#13726,0.309556);
#462=SPHERICAL_SURFACE('',#13731,0.309556);
#463=SPHERICAL_SURFACE('',#13737,0.309556);
#464=SPHERICAL_SURFACE('',#13742,0.309556);
#465=SPHERICAL_SURFACE('',#13747,0.309556);
#466=SPHERICAL_SURFACE('',#13755,0.309556);
#467=CONICAL_SURFACE('',#13234,0.53,0.785398163397448);
#468=CONICAL_SURFACE('',#13241,0.53,0.785398163397448);
#469=CONICAL_SURFACE('',#13254,1.47,0.785398163397449);
#470=CONICAL_SURFACE('',#13258,1.47,0.785398163397449);
#471=CONICAL_SURFACE('',#13642,0.4,0.785398163397448);
#472=CONICAL_SURFACE('',#13646,0.41,0.785398163397448);
#473=CONICAL_SURFACE('',#13650,0.26,0.463647609000806);
#474=CONICAL_SURFACE('',#13666,0.63,0.785398163397448);
#475=CONICAL_SURFACE('',#13673,0.63,0.785398163397448);
#476=CONICAL_SURFACE('',#13686,1.57,0.785398163397449);
#477=CONICAL_SURFACE('',#13690,1.57,0.785398163397449);
#478=CONICAL_SURFACE('',#13794,0.325,0.785398163397448);
#479=CONICAL_SURFACE('',#13798,0.335,0.785398163397448);
#480=CONICAL_SURFACE('',#13802,0.21,0.463647609000806);
#481=CONICAL_SURFACE('',#14336,0.325,0.785398163397448);
#482=CONICAL_SURFACE('',#14340,0.335,0.785398163397448);
#483=CONICAL_SURFACE('',#14344,0.21,0.463647609000806);
#484=CONICAL_SURFACE('',#14348,0.18,0.785398163397448);
#485=CONICAL_SURFACE('',#14472,0.185,0.785398163397449);
#486=CONICAL_SURFACE('',#14476,0.1625,0.785398163397449);
#487=TOROIDAL_SURFACE('',#13223,1.,0.247676);
#488=TOROIDAL_SURFACE('',#13243,1.,0.247676);
#489=TOROIDAL_SURFACE('',#13655,1.1,0.309556);
#490=TOROIDAL_SURFACE('',#13675,1.1,0.309556);
#491=B_SPLINE_CURVE_WITH_KNOTS('',3,(#19153,#19154,#19155,#19156,#19157,
#19158),.UNSPECIFIED.,.F.,.F.,(4,2,4),(1.88587037555333,2.15501811419061,
2.44576925996922),.UNSPECIFIED.);
#492=B_SPLINE_CURVE_WITH_KNOTS('',3,(#19169,#19170,#19171,#19172,#19173,
#19174,#19175,#19176,#19177,#19178,#19179,#19180,#19181,#19182,#19183,#19184,
#19185,#19186,#19187,#19188,#19189,#19190,#19191,#19192,#19193,#19194,#19195,
#19196,#19197,#19198,#19199,#19200),.UNSPECIFIED.,.F.,.F.,(4,2,2,2,2,2,
2,2,2,2,2,2,2,2,2,4),(0.559898884415891,0.581502291557221,0.697930042244281,
0.814357792931341,0.918959320915763,1.02356084890019,1.1232227394424,1.22288462998461,
1.32254652052682,1.42220841106903,1.52680993905346,1.63141146703788,1.74783921772494,
1.864266968412,2.15501811419061,2.44576925996922),.UNSPECIFIED.);
#493=B_SPLINE_CURVE_WITH_KNOTS('',3,(#19203,#19204,#19205,#19206,#19207,
#19208),.UNSPECIFIED.,.F.,.F.,(4,2,4),(0.,0.29075114577861,0.559898884415891),
 .UNSPECIFIED.);
#494=B_SPLINE_CURVE_WITH_KNOTS('',3,(#19217,#19218,#19219,#19220,#19221,
#19222,#19223,#19224,#19225,#19226,#19227,#19228,#19229,#19230,#19231,#19232,
#19233,#19234,#19235,#19236,#19237,#19238,#19239,#19240,#19241,#19242,#19243,
#19244,#19245,#19246,#19247,#19248),.UNSPECIFIED.,.F.,.F.,(4,2,2,2,2,2,
2,2,2,2,2,2,2,2,2,4),(0.,0.29075114577861,0.58150229155722,0.69793004224428,
0.814357792931341,0.918959320915763,1.02356084890019,1.1232227394424,1.22288462998461,
1.32254652052682,1.42220841106904,1.52680993905346,1.63141146703788,1.74783921772494,
1.864266968412,1.88587037555333),.UNSPECIFIED.);
#495=B_SPLINE_CURVE_WITH_KNOTS('',3,(#19542,#19543,#19544,#19545,#19546,
#19547,#19548,#19549,#19550,#19551,#19552,#19553,#19554,#19555,#19556,#19557,
#19558,#19559,#19560,#19561,#19562,#19563),.UNSPECIFIED.,.F.,.F.,(4,2,2,
2,2,2,2,2,2,2,4),(0.0473477652366656,0.126350602536658,0.189525903804987,
0.252701205073317,0.313298422430275,0.373895639787233,0.434492857144191,
0.495090074501149,0.558265375769478,0.621440677037807,0.7004435143378),
 .UNSPECIFIED.);
#496=B_SPLINE_CURVE_WITH_KNOTS('',3,(#19567,#19568,#19569,#19570,#19571,
#19572,#19573,#19574,#19575,#19576,#19577,#19578,#19579,#19580,#19581,#19582,
#19583,#19584,#19585,#19586,#19587,#19588),.UNSPECIFIED.,.F.,.F.,(4,2,2,
2,2,2,2,2,2,2,4),(0.0464897534940957,0.0852567806515119,0.170513561303024,
0.246687263103517,0.308657850341199,0.370628437578881,0.432599024816563,
0.494569612054245,0.570743313854739,0.656000094506251,0.694767121663666),
 .UNSPECIFIED.);
#497=B_SPLINE_CURVE_WITH_KNOTS('',3,(#19594,#19595,#19596,#19597,#19598,
#19599,#19600,#19601,#19602,#19603,#19604,#19605,#19606,#19607,#19608,#19609,
#19610,#19611,#19612,#19613,#19614,#19615),.UNSPECIFIED.,.F.,.F.,(4,2,2,
2,2,2,2,2,2,2,4),(0.0464897534940957,0.0852567806515118,0.170513561303024,
0.246687263103517,0.308657850341199,0.370628437578881,0.432599024816563,
0.494569612054245,0.570743313854738,0.65600009450625,0.694767121663666),
 .UNSPECIFIED.);
#498=B_SPLINE_CURVE_WITH_KNOTS('',3,(#19619,#19620,#19621,#19622,#19623,
#19624,#19625,#19626,#19627,#19628,#19629,#19630,#19631,#19632,#19633,#19634,
#19635,#19636,#19637,#19638,#19639,#19640),.UNSPECIFIED.,.F.,.F.,(4,2,2,
2,2,2,2,2,2,2,4),(0.0464897534940957,0.0852567806515119,0.170513561303024,
0.246687263103517,0.308657850341199,0.370628437578881,0.432599024816563,
0.494569612054245,0.570743313854739,0.656000094506251,0.694767121663666),
 .UNSPECIFIED.);
#499=B_SPLINE_CURVE_WITH_KNOTS('',3,(#19644,#19645,#19646,#19647,#19648,
#19649,#19650,#19651,#19652,#19653,#19654,#19655),.UNSPECIFIED.,.F.,.F.,
(4,2,2,2,2,4),(0.0464897534940957,0.0852567806515119,0.170513561303024,
0.246687263103517,0.308657850341199,0.370628437578881),.UNSPECIFIED.);
#500=B_SPLINE_CURVE_WITH_KNOTS('',3,(#19660,#19661,#19662,#19663,#19664,
#19665,#19666,#19667,#19668,#19669,#19670,#19671),.UNSPECIFIED.,.F.,.F.,
(4,2,2,2,2,4),(0.370628437578881,0.432599024816563,0.494569612054245,0.570743313854738,
0.65600009450625,0.694767121663666),.UNSPECIFIED.);
#501=B_SPLINE_CURVE_WITH_KNOTS('',3,(#19675,#19676,#19677,#19678,#19679,
#19680,#19681,#19682,#19683,#19684,#19685,#19686,#19687,#19688,#19689,#19690,
#19691,#19692,#19693,#19694,#19695,#19696),.UNSPECIFIED.,.F.,.F.,(4,2,2,
2,2,2,2,2,2,2,4),(0.0464897534940957,0.0852567806515121,0.170513561303024,
0.246687263103518,0.308657850341199,0.370628437578881,0.432599024816563,
0.494569612054245,0.570743313854738,0.65600009450625,0.694767121663666),
 .UNSPECIFIED.);
#502=B_SPLINE_CURVE_WITH_KNOTS('',3,(#19700,#19701,#19702,#19703,#19704,
#19705,#19706,#19707,#19708,#19709,#19710,#19711,#19712,#19713,#19714,#19715,
#19716,#19717,#19718,#19719,#19720,#19721),.UNSPECIFIED.,.F.,.F.,(4,2,2,
2,2,2,2,2,2,2,4),(0.0464897534940957,0.0852567806515119,0.170513561303024,
0.246687263103517,0.308657850341199,0.370628437578881,0.432599024816563,
0.494569612054245,0.570743313854738,0.65600009450625,0.694767121663667),
 .UNSPECIFIED.);
#503=B_SPLINE_CURVE_WITH_KNOTS('',3,(#19725,#19726,#19727,#19728,#19729,
#19730,#19731,#19732,#19733,#19734,#19735,#19736,#19737,#19738,#19739,#19740,
#19741,#19742,#19743,#19744,#19745,#19746),.UNSPECIFIED.,.F.,.F.,(4,2,2,
2,2,2,2,2,2,2,4),(0.0464897534940957,0.0852567806515119,0.170513561303024,
0.246687263103517,0.308657850341199,0.370628437578881,0.432599024816563,
0.494569612054245,0.570743313854738,0.65600009450625,0.694767121663666),
 .UNSPECIFIED.);
#504=B_SPLINE_CURVE_WITH_KNOTS('',3,(#19750,#19751,#19752,#19753,#19754,
#19755,#19756,#19757,#19758,#19759,#19760,#19761,#19762,#19763,#19764,#19765,
#19766,#19767,#19768,#19769,#19770,#19771),.UNSPECIFIED.,.F.,.F.,(4,2,2,
2,2,2,2,2,2,2,4),(0.0464897534940957,0.0852567806515119,0.170513561303024,
0.246687263103517,0.308657850341199,0.370628437578881,0.432599024816563,
0.494569612054245,0.570743313854739,0.656000094506251,0.694767121663667),
 .UNSPECIFIED.);
#505=B_SPLINE_CURVE_WITH_KNOTS('',3,(#19779,#19780,#19781,#19782,#19783,
#19784,#19785,#19786,#19787,#19788,#19789,#19790,#19791,#19792,#19793,#19794,
#19795,#19796,#19797,#19798,#19799,#19800),.UNSPECIFIED.,.F.,.F.,(4,2,2,
2,2,2,2,2,2,2,4),(0.0473477652366656,0.126350602536658,0.189525903804987,
0.252701205073316,0.313298422430274,0.373895639787232,0.434492857144191,
0.495090074501149,0.558265375769478,0.621440677037807,0.7004435143378),
 .UNSPECIFIED.);
#506=B_SPLINE_CURVE_WITH_KNOTS('',3,(#19808,#19809,#19810,#19811,#19812,
#19813,#19814,#19815,#19816,#19817,#19818,#19819,#19820,#19821,#19822,#19823,
#19824,#19825,#19826,#19827,#19828,#19829),.UNSPECIFIED.,.F.,.F.,(4,2,2,
2,2,2,2,2,2,2,4),(0.0473477652366656,0.126350602536658,0.189525903804987,
0.252701205073317,0.313298422430275,0.373895639787233,0.434492857144191,
0.495090074501149,0.558265375769478,0.621440677037807,0.7004435143378),
 .UNSPECIFIED.);
#507=B_SPLINE_CURVE_WITH_KNOTS('',3,(#19838,#19839,#19840,#19841,#19842,
#19843,#19844,#19845,#19846,#19847,#19848,#19849),.UNSPECIFIED.,.F.,.F.,
(4,2,2,2,2,4),(0.0473477652366656,0.126350602536658,0.189525903804987,0.252701205073316,
0.313298422430275,0.373895639787233),.UNSPECIFIED.);
#508=B_SPLINE_CURVE_WITH_KNOTS('',3,(#19851,#19852,#19853,#19854,#19855,
#19856,#19857,#19858,#19859,#19860,#19861,#19862),.UNSPECIFIED.,.F.,.F.,
(4,2,2,2,2,4),(0.373895639787233,0.434492857144191,0.495090074501149,0.558265375769478,
0.621440677037807,0.7004435143378),.UNSPECIFIED.);
#509=B_SPLINE_CURVE_WITH_KNOTS('',3,(#19869,#19870,#19871,#19872,#19873,
#19874,#19875,#19876,#19877,#19878,#19879,#19880,#19881,#19882,#19883,#19884,
#19885,#19886,#19887,#19888,#19889,#19890),.UNSPECIFIED.,.F.,.F.,(4,2,2,
2,2,2,2,2,2,2,4),(0.0473477652366656,0.126350602536658,0.189525903804987,
0.252701205073316,0.313298422430275,0.373895639787233,0.434492857144191,
0.495090074501149,0.558265375769478,0.621440677037807,0.7004435143378),
 .UNSPECIFIED.);
#510=B_SPLINE_CURVE_WITH_KNOTS('',3,(#19898,#19899,#19900,#19901,#19902,
#19903,#19904,#19905,#19906,#19907,#19908,#19909,#19910,#19911,#19912,#19913,
#19914,#19915,#19916,#19917,#19918,#19919),.UNSPECIFIED.,.F.,.F.,(4,2,2,
2,2,2,2,2,2,2,4),(0.0473477652366656,0.126350602536658,0.189525903804987,
0.252701205073317,0.313298422430275,0.373895639787233,0.434492857144191,
0.495090074501149,0.558265375769478,0.621440677037807,0.7004435143378),
 .UNSPECIFIED.);
#511=B_SPLINE_CURVE_WITH_KNOTS('',3,(#19927,#19928,#19929,#19930,#19931,
#19932,#19933,#19934,#19935,#19936,#19937,#19938,#19939,#19940,#19941,#19942,
#19943,#19944,#19945,#19946,#19947,#19948),.UNSPECIFIED.,.F.,.F.,(4,2,2,
2,2,2,2,2,2,2,4),(0.0473477652366656,0.126350602536658,0.189525903804987,
0.252701205073316,0.313298422430275,0.373895639787233,0.434492857144191,
0.495090074501149,0.558265375769478,0.621440677037807,0.7004435143378),
 .UNSPECIFIED.);
#512=B_SPLINE_CURVE_WITH_KNOTS('',3,(#19957,#19958,#19959,#19960,#19961,
#19962,#19963,#19964,#19965,#19966,#19967,#19968,#19969,#19970,#19971,#19972,
#19973,#19974,#19975,#19976,#19977,#19978),.UNSPECIFIED.,.F.,.F.,(4,2,2,
2,2,2,2,2,2,2,4),(0.0473477652366656,0.126350602536658,0.189525903804987,
0.252701205073317,0.313298422430275,0.373895639787233,0.434492857144191,
0.495090074501149,0.558265375769478,0.621440677037807,0.7004435143378),
 .UNSPECIFIED.);
#513=B_SPLINE_CURVE_WITH_KNOTS('',3,(#20469,#20470,#20471,#20472,#20473,
#20474),.UNSPECIFIED.,.F.,.F.,(4,2,4),(0.687371506923446,0.701311490231616,
0.764919212052549),.UNSPECIFIED.);
#514=B_SPLINE_CURVE_WITH_KNOTS('',3,(#20478,#20479,#20480,#20481,#20482,
#20483),.UNSPECIFIED.,.F.,.F.,(4,2,4),(0.254973070684183,0.318580792505116,
0.332520775813288),.UNSPECIFIED.);
#515=B_SPLINE_CURVE_WITH_KNOTS('',3,(#20484,#20485,#20486,#20487,#20488,
#20489),.UNSPECIFIED.,.F.,.F.,(4,2,4),(0.177425365555078,0.19136534886325,
0.254973070684183),.UNSPECIFIED.);
#516=B_SPLINE_CURVE_WITH_KNOTS('',3,(#20490,#20491,#20492,#20493,#20494,
#20495),.UNSPECIFIED.,.F.,.F.,(4,2,4),(0.764919212052549,0.828526933873482,
0.842466917181652),.UNSPECIFIED.);
#517=B_SPLINE_CURVE_WITH_KNOTS('',3,(#20953,#20954,#20955,#20956,#20957,
#20958,#20959,#20960,#20961,#20962,#20963,#20964,#20965,#20966,#20967,#20968,
#20969,#20970,#20971,#20972,#20973,#20974),.UNSPECIFIED.,.F.,.F.,(4,2,2,
2,2,2,2,2,2,2,4),(0.0591825211272536,0.157966726598481,0.236950089897721,
0.315933453196962,0.391576304923761,0.46721915665056,0.54286200837736,0.618504860104159,
0.697488223403399,0.77647158670264,0.875255792173867),.UNSPECIFIED.);
#518=B_SPLINE_CURVE_WITH_KNOTS('',3,(#20978,#20979,#20980,#20981,#20982,
#20983,#20984,#20985,#20986,#20987,#20988,#20989,#20990,#20991,#20992,#20993,
#20994,#20995,#20996,#20997,#20998,#20999),.UNSPECIFIED.,.F.,.F.,(4,2,2,
2,2,2,2,2,2,2,4),(0.0581119756758434,0.106553146291161,0.213106292582322,
0.30849933801665,0.386091982889075,0.4636846277615,0.541277272633925,0.61886991750635,
0.714262962940678,0.820816109231839,0.869257279847157),.UNSPECIFIED.);
#519=B_SPLINE_CURVE_WITH_KNOTS('',3,(#21005,#21006,#21007,#21008,#21009,
#21010,#21011,#21012,#21013,#21014,#21015,#21016,#21017,#21018,#21019,#21020,
#21021,#21022,#21023,#21024,#21025,#21026),.UNSPECIFIED.,.F.,.F.,(4,2,2,
2,2,2,2,2,2,2,4),(0.0581119756758434,0.106553146291161,0.213106292582322,
0.30849933801665,0.386091982889075,0.4636846277615,0.541277272633925,0.61886991750635,
0.714262962940679,0.820816109231839,0.869257279847157),.UNSPECIFIED.);
#520=B_SPLINE_CURVE_WITH_KNOTS('',3,(#21030,#21031,#21032,#21033,#21034,
#21035,#21036,#21037,#21038,#21039,#21040,#21041,#21042,#21043,#21044,#21045,
#21046,#21047,#21048,#21049,#21050,#21051),.UNSPECIFIED.,.F.,.F.,(4,2,2,
2,2,2,2,2,2,2,4),(0.0581119756758433,0.106553146291161,0.213106292582322,
0.308499338016649,0.386091982889075,0.4636846277615,0.541277272633925,0.61886991750635,
0.714262962940678,0.820816109231839,0.869257279847157),.UNSPECIFIED.);
#521=B_SPLINE_CURVE_WITH_KNOTS('',3,(#21060,#21061,#21062,#21063,#21064,
#21065,#21066,#21067,#21068,#21069,#21070,#21071,#21072,#21073,#21074,#21075,
#21076,#21077,#21078,#21079,#21080,#21081),.UNSPECIFIED.,.F.,.F.,(4,2,2,
2,2,2,2,2,2,2,4),(0.0581119756758433,0.106553146291161,0.213106292582322,
0.30849933801665,0.386091982889075,0.4636846277615,0.541277272633925,0.61886991750635,
0.714262962940678,0.820816109231839,0.869257279847157),.UNSPECIFIED.);
#522=B_SPLINE_CURVE_WITH_KNOTS('',3,(#21085,#21086,#21087,#21088,#21089,
#21090,#21091,#21092,#21093,#21094,#21095,#21096,#21097,#21098,#21099,#21100,
#21101,#21102,#21103,#21104,#21105,#21106),.UNSPECIFIED.,.F.,.F.,(4,2,2,
2,2,2,2,2,2,2,4),(0.0581119756758434,0.106553146291161,0.213106292582322,
0.30849933801665,0.386091982889075,0.4636846277615,0.541277272633925,0.61886991750635,
0.714262962940678,0.820816109231839,0.869257279847157),.UNSPECIFIED.);
#523=B_SPLINE_CURVE_WITH_KNOTS('',3,(#21110,#21111,#21112,#21113,#21114,
#21115,#21116,#21117,#21118,#21119,#21120,#21121,#21122,#21123,#21124,#21125,
#21126,#21127,#21128,#21129,#21130,#21131),.UNSPECIFIED.,.F.,.F.,(4,2,2,
2,2,2,2,2,2,2,4),(0.0581119756758434,0.106553146291161,0.213106292582322,
0.30849933801665,0.386091982889075,0.4636846277615,0.541277272633925,0.61886991750635,
0.714262962940678,0.820816109231839,0.869257279847157),.UNSPECIFIED.);
#524=B_SPLINE_CURVE_WITH_KNOTS('',3,(#21135,#21136,#21137,#21138,#21139,
#21140,#21141,#21142,#21143,#21144,#21145,#21146,#21147,#21148,#21149,#21150,
#21151,#21152,#21153,#21154,#21155,#21156),.UNSPECIFIED.,.F.,.F.,(4,2,2,
2,2,2,2,2,2,2,4),(0.0581119756758433,0.106553146291161,0.213106292582322,
0.30849933801665,0.386091982889075,0.4636846277615,0.541277272633925,0.61886991750635,
0.714262962940678,0.820816109231839,0.869257279847157),.UNSPECIFIED.);
#525=B_SPLINE_CURVE_WITH_KNOTS('',3,(#21164,#21165,#21166,#21167,#21168,
#21169,#21170,#21171,#21172,#21173,#21174,#21175,#21176,#21177,#21178,#21179,
#21180,#21181,#21182,#21183,#21184,#21185),.UNSPECIFIED.,.F.,.F.,(4,2,2,
2,2,2,2,2,2,2,4),(0.0591825211272536,0.157966726598481,0.236950089897721,
0.315933453196962,0.391576304923761,0.467219156650561,0.54286200837736,
0.618504860104159,0.697488223403399,0.77647158670264,0.875255792173867),
 .UNSPECIFIED.);
#526=B_SPLINE_CURVE_WITH_KNOTS('',3,(#21193,#21194,#21195,#21196,#21197,
#21198,#21199,#21200,#21201,#21202,#21203,#21204,#21205,#21206,#21207,#21208,
#21209,#21210,#21211,#21212,#21213,#21214),.UNSPECIFIED.,.F.,.F.,(4,2,2,
2,2,2,2,2,2,2,4),(0.0591825211272536,0.157966726598481,0.236950089897722,
0.315933453196962,0.391576304923761,0.467219156650561,0.54286200837736,
0.618504860104159,0.697488223403399,0.77647158670264,0.875255792173867),
 .UNSPECIFIED.);
#527=B_SPLINE_CURVE_WITH_KNOTS('',3,(#21224,#21225,#21226,#21227,#21228,
#21229,#21230,#21231,#21232,#21233,#21234,#21235,#21236,#21237,#21238,#21239,
#21240,#21241,#21242,#21243,#21244,#21245),.UNSPECIFIED.,.F.,.F.,(4,2,2,
2,2,2,2,2,2,2,4),(0.0591825211272536,0.157966726598481,0.236950089897721,
0.315933453196962,0.391576304923761,0.46721915665056,0.54286200837736,0.618504860104159,
0.697488223403399,0.77647158670264,0.875255792173867),.UNSPECIFIED.);
#528=B_SPLINE_CURVE_WITH_KNOTS('',3,(#21253,#21254,#21255,#21256,#21257,
#21258,#21259,#21260,#21261,#21262,#21263,#21264,#21265,#21266,#21267,#21268,
#21269,#21270,#21271,#21272,#21273,#21274),.UNSPECIFIED.,.F.,.F.,(4,2,2,
2,2,2,2,2,2,2,4),(0.0591825211272536,0.157966726598481,0.236950089897721,
0.315933453196962,0.391576304923761,0.46721915665056,0.542862008377359,
0.618504860104159,0.697488223403399,0.776471586702639,0.875255792173867),
 .UNSPECIFIED.);
#529=B_SPLINE_CURVE_WITH_KNOTS('',3,(#21282,#21283,#21284,#21285,#21286,
#21287,#21288,#21289,#21290,#21291,#21292,#21293,#21294,#21295,#21296,#21297,
#21298,#21299,#21300,#21301,#21302,#21303),.UNSPECIFIED.,.F.,.F.,(4,2,2,
2,2,2,2,2,2,2,4),(0.0591825211272536,0.157966726598481,0.236950089897721,
0.315933453196962,0.391576304923761,0.46721915665056,0.54286200837736,0.618504860104159,
0.697488223403399,0.77647158670264,0.875255792173867),.UNSPECIFIED.);
#530=B_SPLINE_CURVE_WITH_KNOTS('',3,(#21312,#21313,#21314,#21315,#21316,
#21317,#21318,#21319,#21320,#21321,#21322,#21323,#21324,#21325,#21326,#21327,
#21328,#21329,#21330,#21331,#21332,#21333),.UNSPECIFIED.,.F.,.F.,(4,2,2,
2,2,2,2,2,2,2,4),(0.0591825211272536,0.157966726598481,0.236950089897721,
0.315933453196962,0.391576304923761,0.46721915665056,0.542862008377359,
0.618504860104159,0.697488223403399,0.776471586702639,0.875255792173867),
 .UNSPECIFIED.);
#531=B_SPLINE_CURVE_WITH_KNOTS('',3,(#21553,#21554,#21555,#21556,#21557,
#21558,#21559,#21560,#21561,#21562),.UNSPECIFIED.,.F.,.F.,(4,2,2,2,4),(0.566550474129931,
0.613761886174531,0.66097329821913,0.708186965196186,0.755400632173242),
 .UNSPECIFIED.);
#532=B_SPLINE_CURVE_WITH_KNOTS('',3,(#21564,#21565,#21566,#21567,#21568,
#21569,#21570,#21571,#21572,#21573,#21574,#21575,#21576,#21577,#21578,#21579,
#21580,#21581),.UNSPECIFIED.,.F.,.F.,(4,2,2,2,2,2,2,2,4),(0.18885015804331,
0.23606157008791,0.283272982132509,0.330486649109565,0.377700316086621,
0.424913983063677,0.472127650040732,0.519339062085332,0.566550474129931),
 .UNSPECIFIED.);
#533=B_SPLINE_CURVE_WITH_KNOTS('',3,(#21582,#21583,#21584,#21585,#21586,
#21587,#21588,#21589,#21590,#21591),.UNSPECIFIED.,.F.,.F.,(4,2,2,2,4),(0.755400632173242,
0.802614299150298,0.849827966127353,0.897039378171953,0.944250790216552),
 .UNSPECIFIED.);
#534=B_SPLINE_CURVE_WITH_KNOTS('',3,(#21595,#21596,#21597,#21598,#21599,
#21600,#21601,#21602,#21603,#21604),.UNSPECIFIED.,.F.,.F.,(4,2,2,2,4),(0.189723673274825,
0.237146208024627,0.28456874277443,0.33200804466204,0.37944734654965),
 .UNSPECIFIED.);
#535=B_SPLINE_CURVE_WITH_KNOTS('',3,(#21606,#21607,#21608,#21609,#21610,
#21611,#21612,#21613,#21614,#21615),.UNSPECIFIED.,.F.,.F.,(4,2,2,2,4),(0.,
0.0474393018876097,0.0948786037752193,0.142301138525022,0.189723673274825),
 .UNSPECIFIED.);
#536=B_SPLINE_CURVE_WITH_KNOTS('',3,(#21617,#21618,#21619,#21620,#21621,
#21622,#21623,#21624,#21625,#21626),.UNSPECIFIED.,.F.,.F.,(4,2,2,2,4),(0.569171019824474,
0.616593554574277,0.66401608932408,0.711455391211689,0.758894693099299),
 .UNSPECIFIED.);
#537=B_SPLINE_CURVE_WITH_KNOTS('',3,(#21627,#21628,#21629,#21630,#21631,
#21632,#21633,#21634,#21635,#21636),.UNSPECIFIED.,.F.,.F.,(4,2,2,2,4),(0.37944734654965,
0.426886648437259,0.474325950324869,0.521748485074671,0.569171019824474),
 .UNSPECIFIED.);
#538=B_SPLINE_CURVE_WITH_KNOTS('',3,(#21640,#21641,#21642,#21643,#21644,
#21645,#21646,#21647,#21648,#21649,#21650,#21651,#21652,#21653,#21654,#21655,
#21656,#21657),.UNSPECIFIED.,.F.,.F.,(4,2,2,2,2,2,2,2,4),(0.,0.0474393018876097,
0.0948786037752194,0.142301138525022,0.189723673274825,0.237146208024628,
0.28456874277443,0.33200804466204,0.37944734654965),.UNSPECIFIED.);
#539=B_SPLINE_CURVE_WITH_KNOTS('',3,(#21658,#21659,#21660,#21661,#21662,
#21663,#21664,#21665,#21666,#21667,#21668,#21669,#21670,#21671,#21672,#21673,
#21674,#21675),.UNSPECIFIED.,.F.,.F.,(4,2,2,2,2,2,2,2,4),(0.37944734654965,
0.426886648437259,0.474325950324869,0.521748485074672,0.569171019824474,
0.616593554574277,0.66401608932408,0.711455391211689,0.758894693099299),
 .UNSPECIFIED.);
#540=B_SPLINE_CURVE_WITH_KNOTS('',3,(#21679,#21680,#21681,#21682,#21683,
#21684,#21685,#21686,#21687,#21688),.UNSPECIFIED.,.F.,.F.,(4,2,2,2,4),(0.566550474129931,
0.613761886174531,0.66097329821913,0.708186965196186,0.755400632173242),
 .UNSPECIFIED.);
#541=B_SPLINE_CURVE_WITH_KNOTS('',3,(#21690,#21691,#21692,#21693,#21694,
#21695,#21696,#21697,#21698,#21699,#21700,#21701,#21702,#21703,#21704,#21705,
#21706,#21707),.UNSPECIFIED.,.F.,.F.,(4,2,2,2,2,2,2,2,4),(0.188850158043311,
0.23606157008791,0.283272982132509,0.330486649109565,0.377700316086621,
0.424913983063677,0.472127650040733,0.519339062085332,0.566550474129931),
 .UNSPECIFIED.);
#542=B_SPLINE_CURVE_WITH_KNOTS('',3,(#21708,#21709,#21710,#21711,#21712,
#21713,#21714,#21715,#21716,#21717),.UNSPECIFIED.,.F.,.F.,(4,2,2,2,4),(0.755400632173242,
0.802614299150298,0.849827966127354,0.897039378171953,0.944250790216552),
 .UNSPECIFIED.);
#543=B_SPLINE_CURVE_WITH_KNOTS('',3,(#21727,#21728,#21729,#21730,#21731,
#21732,#21733,#21734,#21735,#21736,#21737,#21738,#21739,#21740,#21741,#21742,
#21743,#21744),.UNSPECIFIED.,.F.,.F.,(4,2,2,2,2,2,2,2,4),(0.18885015804331,
0.23606157008791,0.283272982132509,0.330486649109565,0.377700316086621,
0.424913983063677,0.472127650040732,0.519339062085332,0.566550474129931),
 .UNSPECIFIED.);
#544=B_SPLINE_CURVE_WITH_KNOTS('',3,(#21746,#21747,#21748,#21749,#21750,
#21751,#21752,#21753,#21754,#21755),.UNSPECIFIED.,.F.,.F.,(4,2,2,2,4),(0.566550474129931,
0.613761886174531,0.66097329821913,0.708186965196186,0.755400632173242),
 .UNSPECIFIED.);
#545=B_SPLINE_CURVE_WITH_KNOTS('',3,(#21756,#21757,#21758,#21759,#21760,
#21761,#21762,#21763,#21764,#21765),.UNSPECIFIED.,.F.,.F.,(4,2,2,2,4),(0.755400632173242,
0.802614299150298,0.849827966127353,0.897039378171953,0.944250790216552),
 .UNSPECIFIED.);
#546=B_SPLINE_CURVE_WITH_KNOTS('',3,(#21768,#21769,#21770,#21771,#21772,
#21773,#21774,#21775,#21776,#21777,#21778,#21779,#21780,#21781,#21782,#21783,
#21784,#21785),.UNSPECIFIED.,.F.,.F.,(4,2,2,2,2,2,2,2,4),(0.188850158043311,
0.23606157008791,0.283272982132509,0.330486649109565,0.377700316086621,
0.424913983063677,0.472127650040733,0.519339062085332,0.566550474129932),
 .UNSPECIFIED.);
#547=B_SPLINE_CURVE_WITH_KNOTS('',3,(#21787,#21788,#21789,#21790,#21791,
#21792,#21793,#21794,#21795,#21796),.UNSPECIFIED.,.F.,.F.,(4,2,2,2,4),(0.566550474129932,
0.613761886174531,0.66097329821913,0.708186965196186,0.755400632173242),
 .UNSPECIFIED.);
#548=B_SPLINE_CURVE_WITH_KNOTS('',3,(#21797,#21798,#21799,#21800,#21801,
#21802,#21803,#21804,#21805,#21806),.UNSPECIFIED.,.F.,.F.,(4,2,2,2,4),(0.755400632173242,
0.802614299150298,0.849827966127354,0.897039378171953,0.944250790216552),
 .UNSPECIFIED.);
#549=B_SPLINE_CURVE_WITH_KNOTS('',3,(#21811,#21812,#21813,#21814,#21815,
#21816,#21817,#21818,#21819,#21820,#21821,#21822,#21823,#21824,#21825,#21826,
#21827,#21828),.UNSPECIFIED.,.F.,.F.,(4,2,2,2,2,2,2,2,4),(0.,0.0474393018876097,
0.0948786037752193,0.142301138525022,0.189723673274825,0.237146208024627,
0.28456874277443,0.33200804466204,0.37944734654965),.UNSPECIFIED.);
#550=B_SPLINE_CURVE_WITH_KNOTS('',3,(#21829,#21830,#21831,#21832,#21833,
#21834,#21835,#21836,#21837,#21838,#21839,#21840,#21841,#21842,#21843,#21844,
#21845,#21846),.UNSPECIFIED.,.F.,.F.,(4,2,2,2,2,2,2,2,4),(0.37944734654965,
0.426886648437259,0.474325950324869,0.521748485074672,0.569171019824474,
0.616593554574277,0.66401608932408,0.711455391211689,0.758894693099299),
 .UNSPECIFIED.);
#551=B_SPLINE_CURVE_WITH_KNOTS('',3,(#21850,#21851,#21852,#21853,#21854,
#21855,#21856,#21857,#21858,#21859,#21860,#21861,#21862,#21863,#21864,#21865,
#21866,#21867),.UNSPECIFIED.,.F.,.F.,(4,2,2,2,2,2,2,2,4),(0.,0.0474393018876097,
0.0948786037752194,0.142301138525022,0.189723673274825,0.237146208024627,
0.28456874277443,0.33200804466204,0.37944734654965),.UNSPECIFIED.);
#552=B_SPLINE_CURVE_WITH_KNOTS('',3,(#21868,#21869,#21870,#21871,#21872,
#21873,#21874,#21875,#21876,#21877,#21878,#21879,#21880,#21881,#21882,#21883,
#21884,#21885),.UNSPECIFIED.,.F.,.F.,(4,2,2,2,2,2,2,2,4),(0.37944734654965,
0.426886648437259,0.474325950324869,0.521748485074672,0.569171019824474,
0.616593554574277,0.66401608932408,0.711455391211689,0.758894693099299),
 .UNSPECIFIED.);
#553=B_SPLINE_CURVE_WITH_KNOTS('',3,(#22249,#22250,#22251,#22252,#22253,
#22254,#22255,#22256,#22257,#22258),.UNSPECIFIED.,.F.,.F.,(4,2,2,2,4),(0.565665723963061,
0.61280433739166,0.659942950820258,0.70708195805217,0.754220965284082),
 .UNSPECIFIED.);
#554=B_SPLINE_CURVE_WITH_KNOTS('',3,(#22260,#22261,#22262,#22263,#22264,
#22265,#22266,#22267,#22268,#22269,#22270,#22271,#22272,#22273,#22274,#22275,
#22276,#22277),.UNSPECIFIED.,.F.,.F.,(4,2,2,2,2,2,2,2,4),(0.18855524132102,
0.235693854749619,0.282832468178217,0.329971475410129,0.377110482642041,
0.424249489873953,0.471388497105864,0.518527110534463,0.565665723963061),
 .UNSPECIFIED.);
#555=B_SPLINE_CURVE_WITH_KNOTS('',3,(#22278,#22279,#22280,#22281,#22282,
#22283,#22284,#22285,#22286,#22287),.UNSPECIFIED.,.F.,.F.,(4,2,2,2,4),(0.754220965284082,
0.801359972515993,0.848498979747905,0.895637593176504,0.942776206605102),
 .UNSPECIFIED.);
#556=B_SPLINE_CURVE_WITH_KNOTS('',3,(#22291,#22292,#22293,#22294,#22295,
#22296,#22297,#22298,#22299,#22300),.UNSPECIFIED.,.F.,.F.,(4,2,2,2,4),(0.188940047579712,
0.236173496177583,0.283406944775455,0.330643519967439,0.377880095159423),
 .UNSPECIFIED.);
#557=B_SPLINE_CURVE_WITH_KNOTS('',3,(#22302,#22303,#22304,#22305,#22306,
#22307,#22308,#22309,#22310,#22311),.UNSPECIFIED.,.F.,.F.,(4,2,2,2,4),(0.,
0.0472365751919841,0.0944731503839682,0.14170659898184,0.188940047579712),
 .UNSPECIFIED.);
#558=B_SPLINE_CURVE_WITH_KNOTS('',3,(#22313,#22314,#22315,#22316,#22317,
#22318,#22319,#22320,#22321,#22322),.UNSPECIFIED.,.F.,.F.,(4,2,2,2,4),(0.566820142739135,
0.614053591337007,0.661287039934879,0.708523615126863,0.755760190318847),
 .UNSPECIFIED.);
#559=B_SPLINE_CURVE_WITH_KNOTS('',3,(#22323,#22324,#22325,#22326,#22327,
#22328,#22329,#22330,#22331,#22332),.UNSPECIFIED.,.F.,.F.,(4,2,2,2,4),(0.377880095159423,
0.425116670351408,0.472353245543392,0.519586694141263,0.566820142739135),
 .UNSPECIFIED.);
#560=B_SPLINE_CURVE_WITH_KNOTS('',3,(#22336,#22337,#22338,#22339,#22340,
#22341,#22342,#22343,#22344,#22345,#22346,#22347,#22348,#22349,#22350,#22351,
#22352,#22353),.UNSPECIFIED.,.F.,.F.,(4,2,2,2,2,2,2,2,4),(0.,0.0472365751919841,
0.0944731503839683,0.14170659898184,0.188940047579712,0.236173496177583,
0.283406944775455,0.330643519967439,0.377880095159423),.UNSPECIFIED.);
#561=B_SPLINE_CURVE_WITH_KNOTS('',3,(#22354,#22355,#22356,#22357,#22358,
#22359,#22360,#22361,#22362,#22363,#22364,#22365,#22366,#22367,#22368,#22369,
#22370,#22371),.UNSPECIFIED.,.F.,.F.,(4,2,2,2,2,2,2,2,4),(0.377880095159423,
0.425116670351408,0.472353245543392,0.519586694141263,0.566820142739135,
0.614053591337007,0.661287039934879,0.708523615126863,0.755760190318847),
 .UNSPECIFIED.);
#562=B_SPLINE_CURVE_WITH_KNOTS('',3,(#22375,#22376,#22377,#22378,#22379,
#22380,#22381,#22382,#22383,#22384),.UNSPECIFIED.,.F.,.F.,(4,2,2,2,4),(0.565665723963061,
0.61280433739166,0.659942950820258,0.70708195805217,0.754220965284082),
 .UNSPECIFIED.);
#563=B_SPLINE_CURVE_WITH_KNOTS('',3,(#22386,#22387,#22388,#22389,#22390,
#22391,#22392,#22393,#22394,#22395,#22396,#22397,#22398,#22399,#22400,#22401,
#22402,#22403),.UNSPECIFIED.,.F.,.F.,(4,2,2,2,2,2,2,2,4),(0.18855524132102,
0.235693854749619,0.282832468178217,0.329971475410129,0.377110482642041,
0.424249489873953,0.471388497105864,0.518527110534463,0.565665723963061),
 .UNSPECIFIED.);
#564=B_SPLINE_CURVE_WITH_KNOTS('',3,(#22404,#22405,#22406,#22407,#22408,
#22409,#22410,#22411,#22412,#22413),.UNSPECIFIED.,.F.,.F.,(4,2,2,2,4),(0.754220965284082,
0.801359972515993,0.848498979747905,0.895637593176504,0.942776206605102),
 .UNSPECIFIED.);
#565=B_SPLINE_CURVE_WITH_KNOTS('',3,(#22423,#22424,#22425,#22426,#22427,
#22428,#22429,#22430,#22431,#22432,#22433,#22434,#22435,#22436,#22437,#22438,
#22439,#22440),.UNSPECIFIED.,.F.,.F.,(4,2,2,2,2,2,2,2,4),(0.18855524132102,
0.235693854749619,0.282832468178217,0.329971475410129,0.377110482642041,
0.424249489873953,0.471388497105864,0.518527110534463,0.565665723963061),
 .UNSPECIFIED.);
#566=B_SPLINE_CURVE_WITH_KNOTS('',3,(#22442,#22443,#22444,#22445,#22446,
#22447,#22448,#22449,#22450,#22451),.UNSPECIFIED.,.F.,.F.,(4,2,2,2,4),(0.565665723963061,
0.61280433739166,0.659942950820258,0.70708195805217,0.754220965284082),
 .UNSPECIFIED.);
#567=B_SPLINE_CURVE_WITH_KNOTS('',3,(#22452,#22453,#22454,#22455,#22456,
#22457,#22458,#22459,#22460,#22461),.UNSPECIFIED.,.F.,.F.,(4,2,2,2,4),(0.754220965284082,
0.801359972515993,0.848498979747905,0.895637593176504,0.942776206605102),
 .UNSPECIFIED.);
#568=B_SPLINE_CURVE_WITH_KNOTS('',3,(#22464,#22465,#22466,#22467,#22468,
#22469,#22470,#22471,#22472,#22473,#22474,#22475,#22476,#22477,#22478,#22479,
#22480,#22481),.UNSPECIFIED.,.F.,.F.,(4,2,2,2,2,2,2,2,4),(0.18855524132102,
0.235693854749619,0.282832468178217,0.329971475410129,0.377110482642041,
0.424249489873953,0.471388497105864,0.518527110534463,0.565665723963061),
 .UNSPECIFIED.);
#569=B_SPLINE_CURVE_WITH_KNOTS('',3,(#22483,#22484,#22485,#22486,#22487,
#22488,#22489,#22490,#22491,#22492),.UNSPECIFIED.,.F.,.F.,(4,2,2,2,4),(0.565665723963061,
0.61280433739166,0.659942950820258,0.70708195805217,0.754220965284082),
 .UNSPECIFIED.);
#570=B_SPLINE_CURVE_WITH_KNOTS('',3,(#22493,#22494,#22495,#22496,#22497,
#22498,#22499,#22500,#22501,#22502),.UNSPECIFIED.,.F.,.F.,(4,2,2,2,4),(0.754220965284082,
0.801359972515993,0.848498979747905,0.895637593176504,0.942776206605102),
 .UNSPECIFIED.);
#571=B_SPLINE_CURVE_WITH_KNOTS('',3,(#22507,#22508,#22509,#22510,#22511,
#22512,#22513,#22514,#22515,#22516,#22517,#22518,#22519,#22520,#22521,#22522,
#22523,#22524),.UNSPECIFIED.,.F.,.F.,(4,2,2,2,2,2,2,2,4),(0.,0.0472365751919841,
0.0944731503839683,0.14170659898184,0.188940047579712,0.236173496177583,
0.283406944775455,0.330643519967439,0.377880095159424),.UNSPECIFIED.);
#572=B_SPLINE_CURVE_WITH_KNOTS('',3,(#22525,#22526,#22527,#22528,#22529,
#22530,#22531,#22532,#22533,#22534,#22535,#22536,#22537,#22538,#22539,#22540,
#22541,#22542),.UNSPECIFIED.,.F.,.F.,(4,2,2,2,2,2,2,2,4),(0.377880095159424,
0.425116670351408,0.472353245543392,0.519586694141263,0.566820142739135,
0.614053591337007,0.661287039934879,0.708523615126863,0.755760190318847),
 .UNSPECIFIED.);
#573=B_SPLINE_CURVE_WITH_KNOTS('',3,(#22546,#22547,#22548,#22549,#22550,
#22551,#22552,#22553,#22554,#22555,#22556,#22557,#22558,#22559,#22560,#22561,
#22562,#22563),.UNSPECIFIED.,.F.,.F.,(4,2,2,2,2,2,2,2,4),(0.,0.0472365751919841,
0.0944731503839683,0.14170659898184,0.188940047579712,0.236173496177583,
0.283406944775455,0.330643519967439,0.377880095159423),.UNSPECIFIED.);
#574=B_SPLINE_CURVE_WITH_KNOTS('',3,(#22564,#22565,#22566,#22567,#22568,
#22569,#22570,#22571,#22572,#22573,#22574,#22575,#22576,#22577,#22578,#22579,
#22580,#22581),.UNSPECIFIED.,.F.,.F.,(4,2,2,2,2,2,2,2,4),(0.377880095159423,
0.425116670351408,0.472353245543392,0.519586694141263,0.566820142739135,
0.614053591337007,0.661287039934879,0.708523615126863,0.755760190318847),
 .UNSPECIFIED.);
#575=B_SPLINE_CURVE_WITH_KNOTS('',3,(#23279,#23280,#23281,#23282,#23283,
#23284),.UNSPECIFIED.,.F.,.F.,(4,2,4),(0.665271585430997,0.692803751398642,
0.755746158887618),.UNSPECIFIED.);
#576=B_SPLINE_CURVE_WITH_KNOTS('',3,(#23288,#23289,#23290,#23291,#23292,
#23293),.UNSPECIFIED.,.F.,.F.,(4,2,4),(0.251915386295873,0.31485779378485,
0.342389959752494),.UNSPECIFIED.);
#577=B_SPLINE_CURVE_WITH_KNOTS('',3,(#23294,#23295,#23296,#23297,#23298,
#23299),.UNSPECIFIED.,.F.,.F.,(4,2,4),(0.161440812839248,0.188972978806896,
0.251915386295873),.UNSPECIFIED.);
#578=B_SPLINE_CURVE_WITH_KNOTS('',3,(#23300,#23301,#23302,#23303,#23304,
#23305),.UNSPECIFIED.,.F.,.F.,(4,2,4),(0.755746158887618,0.818688566376595,
0.84622073234424),.UNSPECIFIED.);
#579=B_SPLINE_CURVE_WITH_KNOTS('',3,(#23309,#23310,#23311,#23312,#23313,
#23314,#23315,#23316,#23317,#23318),.UNSPECIFIED.,.F.,.F.,(4,2,2,2,4),(0.,
0.0622075173149514,0.124415034629903,0.186622241324509,0.248829448019115),
 .UNSPECIFIED.);
#580=B_SPLINE_CURVE_WITH_KNOTS('',3,(#23320,#23321,#23322,#23323,#23324,
#23325,#23326,#23327,#23328,#23329),.UNSPECIFIED.,.F.,.F.,(4,2,2,2,4),(0.746488344057344,
0.80869555075195,0.870902757446556,0.933110274761507,0.995317792076459),
 .UNSPECIFIED.);
#581=B_SPLINE_CURVE_WITH_KNOTS('',3,(#23330,#23331,#23332,#23333,#23334,
#23335,#23336,#23337,#23338,#23339,#23340,#23341,#23342,#23343,#23344,#23345,
#23346,#23347),.UNSPECIFIED.,.F.,.F.,(4,2,2,2,2,2,2,2,4),(0.248829448019115,
0.311036654713721,0.373243861408327,0.435451378723278,0.497658896038229,
0.559866413353181,0.622073930668132,0.684281137362738,0.746488344057344),
 .UNSPECIFIED.);
#582=SHAPE_REPRESENTATION_RELATIONSHIP('SRR','None',#23827,#637);
#583=SHAPE_REPRESENTATION_RELATIONSHIP('SRR','None',#23828,#638);
#584=SHAPE_REPRESENTATION_RELATIONSHIP('SRR','None',#23829,#639);
#585=SHAPE_REPRESENTATION_RELATIONSHIP('SRR','None',#23830,#640);
#586=SHAPE_REPRESENTATION_RELATIONSHIP('SRR','None',#23831,#641);
#587=SHAPE_REPRESENTATION_RELATIONSHIP('SRR','None',#23832,#642);
#588=SHAPE_REPRESENTATION_RELATIONSHIP('SRR','None',#23833,#643);
#589=SHAPE_REPRESENTATION_RELATIONSHIP('SRR','None',#23834,#644);
#590=SHAPE_REPRESENTATION_RELATIONSHIP('SRR','None',#23835,#645);
#591=SHAPE_REPRESENTATION_RELATIONSHIP('SRR','None',#23836,#646);
#592=SHAPE_REPRESENTATION_RELATIONSHIP('SRR','None',#23837,#647);
#593=SHAPE_REPRESENTATION_RELATIONSHIP('SRR','None',#23838,#648);
#594=SHAPE_REPRESENTATION_RELATIONSHIP('SRR','None',#23839,#649);
#595=SHAPE_REPRESENTATION_RELATIONSHIP('SRR','None',#23840,#650);
#596=SHAPE_REPRESENTATION_RELATIONSHIP('SRR','None',#23842,#651);
#597=SHAPE_REPRESENTATION_RELATIONSHIP('SRR','None',#23843,#652);
#598=SHAPE_REPRESENTATION_RELATIONSHIP('SRR','None',#23844,#653);
#599=SHAPE_REPRESENTATION_RELATIONSHIP('SRR','None',#23845,#654);
#600=SHAPE_REPRESENTATION_RELATIONSHIP('SRR','None',#23846,#655);
#601=SHAPE_REPRESENTATION_RELATIONSHIP('SRR','None',#23848,#656);
#602=SHAPE_REPRESENTATION_RELATIONSHIP('SRR','None',#23849,#657);
#603=SHAPE_REPRESENTATION_RELATIONSHIP('SRR','None',#23850,#658);
#604=SHAPE_REPRESENTATION_RELATIONSHIP('SRR','None',#23851,#659);
#605=SHAPE_REPRESENTATION_RELATIONSHIP('SRR','None',#23852,#660);
#606=SHAPE_REPRESENTATION_RELATIONSHIP('SRR','None',#23853,#661);
#607=SHAPE_REPRESENTATION_RELATIONSHIP('SRR','None',#23854,#662);
#608=SHAPE_REPRESENTATION_RELATIONSHIP('SRR','None',#23855,#663);
#609=SHAPE_REPRESENTATION_RELATIONSHIP('SRR','None',#23857,#664);
#610=SHAPE_REPRESENTATION_RELATIONSHIP('SRR','None',#23858,#665);
#611=SHAPE_REPRESENTATION_RELATIONSHIP('SRR','None',#23859,#666);
#612=SHAPE_REPRESENTATION_RELATIONSHIP('SRR','None',#23860,#667);
#613=SHAPE_REPRESENTATION_RELATIONSHIP('SRR','None',#23862,#668);
#614=SHAPE_REPRESENTATION_RELATIONSHIP('SRR','None',#23863,#669);
#615=SHAPE_REPRESENTATION_RELATIONSHIP('SRR','None',#23864,#670);
#616=SHAPE_REPRESENTATION_RELATIONSHIP('SRR','None',#23865,#671);
#617=SHAPE_REPRESENTATION_RELATIONSHIP('SRR','None',#23866,#672);
#618=SHAPE_REPRESENTATION_RELATIONSHIP('SRR','None',#23867,#673);
#619=SHAPE_REPRESENTATION_RELATIONSHIP('SRR','None',#23869,#674);
#620=SHAPE_REPRESENTATION_RELATIONSHIP('SRR','None',#23870,#675);
#621=SHAPE_REPRESENTATION_RELATIONSHIP('SRR','None',#23871,#676);
#622=SHAPE_REPRESENTATION_RELATIONSHIP('SRR','None',#23872,#677);
#623=SHAPE_REPRESENTATION_RELATIONSHIP('SRR','None',#23873,#678);
#624=SHAPE_REPRESENTATION_RELATIONSHIP('SRR','None',#23874,#679);
#625=SHAPE_REPRESENTATION_RELATIONSHIP('SRR','None',#23875,#680);
#626=SHAPE_REPRESENTATION_RELATIONSHIP('SRR','None',#23877,#681);
#627=SHAPE_REPRESENTATION_RELATIONSHIP('SRR','None',#23878,#682);
#628=SHAPE_REPRESENTATION_RELATIONSHIP('SRR','None',#23879,#683);
#629=SHAPE_REPRESENTATION_RELATIONSHIP('SRR','None',#23880,#684);
#630=SHAPE_REPRESENTATION_RELATIONSHIP('SRR','None',#23881,#685);
#631=SHAPE_REPRESENTATION_RELATIONSHIP('SRR','None',#23882,#686);
#632=SHAPE_REPRESENTATION_RELATIONSHIP('SRR','None',#23883,#687);
#633=SHAPE_REPRESENTATION_RELATIONSHIP('SRR','None',#23884,#688);
#634=SHAPE_REPRESENTATION_RELATIONSHIP('SRR','None',#23886,#689);
#635=SHAPE_REPRESENTATION_RELATIONSHIP('SRR','None',#23887,#690);
#636=SHAPE_REPRESENTATION_RELATIONSHIP('SRR','None',#23888,#691);
#637=ADVANCED_BREP_SHAPE_REPRESENTATION('',(#762),#23525);
#638=ADVANCED_BREP_SHAPE_REPRESENTATION('',(#763),#23526);
#639=ADVANCED_BREP_SHAPE_REPRESENTATION('',(#764),#23527);
#640=ADVANCED_BREP_SHAPE_REPRESENTATION('',(#765),#23528);
#641=ADVANCED_BREP_SHAPE_REPRESENTATION('',(#766),#23529);
#642=ADVANCED_BREP_SHAPE_REPRESENTATION('',(#767),#23530);
#643=ADVANCED_BREP_SHAPE_REPRESENTATION('',(#768),#23531);
#644=ADVANCED_BREP_SHAPE_REPRESENTATION('',(#769),#23532);
#645=ADVANCED_BREP_SHAPE_REPRESENTATION('',(#770),#23533);
#646=ADVANCED_BREP_SHAPE_REPRESENTATION('',(#771),#23534);
#647=ADVANCED_BREP_SHAPE_REPRESENTATION('',(#772),#23535);
#648=ADVANCED_BREP_SHAPE_REPRESENTATION('',(#773),#23536);
#649=ADVANCED_BREP_SHAPE_REPRESENTATION('',(#774),#23537);
#650=ADVANCED_BREP_SHAPE_REPRESENTATION('',(#775),#23538);
#651=ADVANCED_BREP_SHAPE_REPRESENTATION('',(#776),#23540);
#652=ADVANCED_BREP_SHAPE_REPRESENTATION('',(#777),#23541);
#653=ADVANCED_BREP_SHAPE_REPRESENTATION('',(#778,#779,#780,#781,#782,#783,
#784,#785),#23542);
#654=ADVANCED_BREP_SHAPE_REPRESENTATION('',(#786),#23543);
#655=ADVANCED_BREP_SHAPE_REPRESENTATION('',(#787,#788),#23544);
#656=ADVANCED_BREP_SHAPE_REPRESENTATION('',(#789),#23546);
#657=ADVANCED_BREP_SHAPE_REPRESENTATION('',(#790),#23547);
#658=ADVANCED_BREP_SHAPE_REPRESENTATION('',(#791),#23548);
#659=ADVANCED_BREP_SHAPE_REPRESENTATION('',(#792),#23549);
#660=ADVANCED_BREP_SHAPE_REPRESENTATION('',(#793),#23550);
#661=ADVANCED_BREP_SHAPE_REPRESENTATION('',(#794),#23551);
#662=ADVANCED_BREP_SHAPE_REPRESENTATION('',(#795),#23552);
#663=ADVANCED_BREP_SHAPE_REPRESENTATION('',(#796),#23553);
#664=ADVANCED_BREP_SHAPE_REPRESENTATION('',(#797),#23555);
#665=ADVANCED_BREP_SHAPE_REPRESENTATION('',(#798),#23556);
#666=ADVANCED_BREP_SHAPE_REPRESENTATION('',(#799),#23557);
#667=ADVANCED_BREP_SHAPE_REPRESENTATION('',(#14),#23558);
#668=ADVANCED_BREP_SHAPE_REPRESENTATION('',(#800),#23560);
#669=ADVANCED_BREP_SHAPE_REPRESENTATION('',(#801),#23561);
#670=ADVANCED_BREP_SHAPE_REPRESENTATION('',(#802,#803,#804,#805,#806,#807,
#808),#23562);
#671=ADVANCED_BREP_SHAPE_REPRESENTATION('',(#809),#23563);
#672=ADVANCED_BREP_SHAPE_REPRESENTATION('',(#810,#811),#23564);
#673=ADVANCED_BREP_SHAPE_REPRESENTATION('',(#15),#23565);
#674=ADVANCED_BREP_SHAPE_REPRESENTATION('',(#812),#23567);
#675=ADVANCED_BREP_SHAPE_REPRESENTATION('',(#813),#23568);
#676=ADVANCED_BREP_SHAPE_REPRESENTATION('',(#814),#23569);
#677=ADVANCED_BREP_SHAPE_REPRESENTATION('',(#815),#23570);
#678=ADVANCED_BREP_SHAPE_REPRESENTATION('',(#816),#23571);
#679=ADVANCED_BREP_SHAPE_REPRESENTATION('',(#817),#23572);
#680=ADVANCED_BREP_SHAPE_REPRESENTATION('',(#818),#23573);
#681=ADVANCED_BREP_SHAPE_REPRESENTATION('',(#819),#23575);
#682=ADVANCED_BREP_SHAPE_REPRESENTATION('',(#820),#23576);
#683=ADVANCED_BREP_SHAPE_REPRESENTATION('',(#821),#23577);
#684=ADVANCED_BREP_SHAPE_REPRESENTATION('',(#822),#23578);
#685=ADVANCED_BREP_SHAPE_REPRESENTATION('',(#823),#23579);
#686=ADVANCED_BREP_SHAPE_REPRESENTATION('',(#824),#23580);
#687=ADVANCED_BREP_SHAPE_REPRESENTATION('',(#825),#23581);
#688=ADVANCED_BREP_SHAPE_REPRESENTATION('',(#16),#23582);
#689=ADVANCED_BREP_SHAPE_REPRESENTATION('',(#826),#23584);
#690=ADVANCED_BREP_SHAPE_REPRESENTATION('',(#827),#23585);
#691=ADVANCED_BREP_SHAPE_REPRESENTATION('',(#828),#23586);
#692=STYLED_ITEM('',(#24190),#762);
#693=STYLED_ITEM('',(#24225),#763);
#694=STYLED_ITEM('',(#24225),#764);
#695=STYLED_ITEM('',(#24211),#765);
#696=STYLED_ITEM('',(#24204),#766);
#697=STYLED_ITEM('',(#24211),#767);
#698=STYLED_ITEM('',(#24211),#768);
#699=STYLED_ITEM('',(#24218),#769);
#700=STYLED_ITEM('',(#24218),#770);
#701=STYLED_ITEM('',(#24218),#771);
#702=STYLED_ITEM('',(#24218),#772);
#703=STYLED_ITEM('',(#24225),#773);
#704=STYLED_ITEM('',(#24197),#774);
#705=STYLED_ITEM('',(#24204),#775);
#706=STYLED_ITEM('',(#24211),#776);
#707=STYLED_ITEM('',(#24211),#777);
#708=STYLED_ITEM('',(#24211),#778);
#709=STYLED_ITEM('',(#24211),#779);
#710=STYLED_ITEM('',(#24211),#780);
#711=STYLED_ITEM('',(#24211),#781);
#712=STYLED_ITEM('',(#24211),#782);
#713=STYLED_ITEM('',(#24211),#783);
#714=STYLED_ITEM('',(#24211),#784);
#715=STYLED_ITEM('',(#24211),#785);
#716=STYLED_ITEM('',(#24211),#786);
#717=STYLED_ITEM('',(#24211),#787);
#718=STYLED_ITEM('',(#24211),#788);
#719=STYLED_ITEM('',(#24197),#789);
#720=STYLED_ITEM('',(#24211),#790);
#721=STYLED_ITEM('',(#24225),#791);
#722=STYLED_ITEM('',(#24211),#792);
#723=STYLED_ITEM('',(#24211),#793);
#724=STYLED_ITEM('',(#24218),#794);
#725=STYLED_ITEM('',(#24211),#795);
#726=STYLED_ITEM('',(#24211),#796);
#727=STYLED_ITEM('',(#24190),#797);
#728=STYLED_ITEM('',(#24204),#798);
#729=STYLED_ITEM('',(#24225),#799);
#730=STYLED_ITEM('',(#24218),#14);
#731=STYLED_ITEM('',(#24211),#800);
#732=STYLED_ITEM('',(#24211),#801);
#733=STYLED_ITEM('',(#24211),#802);
#734=STYLED_ITEM('',(#24211),#803);
#735=STYLED_ITEM('',(#24211),#804);
#736=STYLED_ITEM('',(#24211),#805);
#737=STYLED_ITEM('',(#24211),#806);
#738=STYLED_ITEM('',(#24211),#807);
#739=STYLED_ITEM('',(#24211),#808);
#740=STYLED_ITEM('',(#24211),#809);
#741=STYLED_ITEM('',(#24211),#810);
#742=STYLED_ITEM('',(#24211),#811);
#743=STYLED_ITEM('',(#24218),#15);
#744=STYLED_ITEM('',(#24211),#812);
#745=STYLED_ITEM('',(#24225),#813);
#746=STYLED_ITEM('',(#24197),#814);
#747=STYLED_ITEM('',(#24218),#815);
#748=STYLED_ITEM('',(#24218),#816);
#749=STYLED_ITEM('',(#24204),#817);
#750=STYLED_ITEM('',(#24225),#818);
#751=STYLED_ITEM('',(#24211),#819);
#752=STYLED_ITEM('',(#24204),#820);
#753=STYLED_ITEM('',(#24204),#821);
#754=STYLED_ITEM('',(#24218),#822);
#755=STYLED_ITEM('',(#24218),#823);
#756=STYLED_ITEM('',(#24225),#824);
#757=STYLED_ITEM('',(#24204),#825);
#758=STYLED_ITEM('',(#24218),#16);
#759=STYLED_ITEM('',(#24197),#826);
#760=STYLED_ITEM('',(#24197),#827);
#761=STYLED_ITEM('',(#24218),#828);
#762=MANIFOLD_SOLID_BREP('Body1',#12197);
#763=MANIFOLD_SOLID_BREP('Body1',#12198);
#764=MANIFOLD_SOLID_BREP('Body1',#12199);
#765=MANIFOLD_SOLID_BREP('Body1',#12200);
#766=MANIFOLD_SOLID_BREP('Body1',#12201);
#767=MANIFOLD_SOLID_BREP('Body1',#12202);
#768=MANIFOLD_SOLID_BREP('Body1',#12203);
#769=MANIFOLD_SOLID_BREP('Body1',#12204);
#770=MANIFOLD_SOLID_BREP('Body1',#12205);
#771=MANIFOLD_SOLID_BREP('Body1',#12206);
#772=MANIFOLD_SOLID_BREP('Body1',#12207);
#773=MANIFOLD_SOLID_BREP('Body1',#12208);
#774=MANIFOLD_SOLID_BREP('Body1',#12209);
#775=MANIFOLD_SOLID_BREP('Body1',#12210);
#776=MANIFOLD_SOLID_BREP('Body1',#12211);
#777=MANIFOLD_SOLID_BREP('Body1',#12212);
#778=MANIFOLD_SOLID_BREP('Body1',#12213);
#779=MANIFOLD_SOLID_BREP('Body2',#12214);
#780=MANIFOLD_SOLID_BREP('Body3',#12215);
#781=MANIFOLD_SOLID_BREP('Body4',#12216);
#782=MANIFOLD_SOLID_BREP('Body5',#12217);
#783=MANIFOLD_SOLID_BREP('Body6',#12218);
#784=MANIFOLD_SOLID_BREP('Body7',#12219);
#785=MANIFOLD_SOLID_BREP('Body8',#12220);
#786=MANIFOLD_SOLID_BREP('Continuous crown cage',#12221);
#787=MANIFOLD_SOLID_BREP('Body1',#12222);
#788=MANIFOLD_SOLID_BREP('Body2',#12223);
#789=MANIFOLD_SOLID_BREP('Body1',#12224);
#790=MANIFOLD_SOLID_BREP('Body1',#12225);
#791=MANIFOLD_SOLID_BREP('Body1',#12226);
#792=MANIFOLD_SOLID_BREP('Body1',#12227);
#793=MANIFOLD_SOLID_BREP('Body1',#12228);
#794=MANIFOLD_SOLID_BREP('Body1',#12229);
#795=MANIFOLD_SOLID_BREP('Body1',#12230);
#796=MANIFOLD_SOLID_BREP('Body1',#12231);
#797=MANIFOLD_SOLID_BREP('Body1',#12232);
#798=MANIFOLD_SOLID_BREP('Body1',#12233);
#799=MANIFOLD_SOLID_BREP('Body1',#12234);
#800=MANIFOLD_SOLID_BREP('Body1',#12237);
#801=MANIFOLD_SOLID_BREP('Body1',#12238);
#802=MANIFOLD_SOLID_BREP('Body1',#12239);
#803=MANIFOLD_SOLID_BREP('Body2',#12240);
#804=MANIFOLD_SOLID_BREP('Body3',#12241);
#805=MANIFOLD_SOLID_BREP('Body4',#12242);
#806=MANIFOLD_SOLID_BREP('Body5',#12243);
#807=MANIFOLD_SOLID_BREP('Body6',#12244);
#808=MANIFOLD_SOLID_BREP('Body7',#12245);
#809=MANIFOLD_SOLID_BREP('Continuous crown cage',#12246);
#810=MANIFOLD_SOLID_BREP('Body1',#12247);
#811=MANIFOLD_SOLID_BREP('Body2',#12248);
#812=MANIFOLD_SOLID_BREP('Body1',#12251);
#813=MANIFOLD_SOLID_BREP('Body1',#12252);
#814=MANIFOLD_SOLID_BREP('Body1',#12253);
#815=MANIFOLD_SOLID_BREP('Body1',#12254);
#816=MANIFOLD_SOLID_BREP('Body1',#12255);
#817=MANIFOLD_SOLID_BREP('Body1',#12256);
#818=MANIFOLD_SOLID_BREP('Body1',#12257);
#819=MANIFOLD_SOLID_BREP('Body1',#12258);
#820=MANIFOLD_SOLID_BREP('Body1',#12259);
#821=MANIFOLD_SOLID_BREP('Body1',#12260);
#822=MANIFOLD_SOLID_BREP('Body1',#12261);
#823=MANIFOLD_SOLID_BREP('Body1',#12262);
#824=MANIFOLD_SOLID_BREP('Body1',#12263);
#825=MANIFOLD_SOLID_BREP('Body1',#12264);
#826=MANIFOLD_SOLID_BREP('Body1',#12267);
#827=MANIFOLD_SOLID_BREP('Body1',#12268);
#828=MANIFOLD_SOLID_BREP('Body1',#12269);
#829=FACE_BOUND('',#2089,.T.);
#830=FACE_BOUND('',#2090,.T.);
#831=FACE_BOUND('',#2091,.T.);
#832=FACE_BOUND('',#2092,.T.);
#833=FACE_BOUND('',#2093,.T.);
#834=FACE_BOUND('',#2094,.T.);
#835=FACE_BOUND('',#2095,.T.);
#836=FACE_BOUND('',#2096,.T.);
#837=FACE_BOUND('',#2097,.T.);
#838=FACE_BOUND('',#2098,.T.);
#839=FACE_BOUND('',#2099,.T.);
#840=FACE_BOUND('',#2100,.T.);
#841=FACE_BOUND('',#2101,.T.);
#842=FACE_BOUND('',#2102,.T.);
#843=FACE_BOUND('',#2126,.T.);
#844=FACE_BOUND('',#2127,.T.);
#845=FACE_BOUND('',#2129,.T.);
#846=FACE_BOUND('',#2130,.T.);
#847=FACE_BOUND('',#2134,.T.);
#848=FACE_BOUND('',#2135,.T.);
#849=FACE_BOUND('',#2136,.T.);
#850=FACE_BOUND('',#2137,.T.);
#851=FACE_BOUND('',#2138,.T.);
#852=FACE_BOUND('',#2141,.T.);
#853=FACE_BOUND('',#2142,.T.);
#854=FACE_BOUND('',#2143,.T.);
#855=FACE_BOUND('',#2144,.T.);
#856=FACE_BOUND('',#2145,.T.);
#857=FACE_BOUND('',#2149,.T.);
#858=FACE_BOUND('',#2150,.T.);
#859=FACE_BOUND('',#2151,.T.);
#860=FACE_BOUND('',#2152,.T.);
#861=FACE_BOUND('',#2156,.T.);
#862=FACE_BOUND('',#2158,.T.);
#863=FACE_BOUND('',#2164,.T.);
#864=FACE_BOUND('',#2171,.T.);
#865=FACE_BOUND('',#2174,.T.);
#866=FACE_BOUND('',#2180,.T.);
#867=FACE_BOUND('',#2187,.T.);
#868=FACE_BOUND('',#2190,.T.);
#869=FACE_BOUND('',#2193,.T.);
#870=FACE_BOUND('',#2196,.T.);
#871=FACE_BOUND('',#2202,.T.);
#872=FACE_BOUND('',#2205,.T.);
#873=FACE_BOUND('',#2207,.T.);
#874=FACE_BOUND('',#2208,.T.);
#875=FACE_BOUND('',#2210,.T.);
#876=FACE_BOUND('',#2211,.T.);
#877=FACE_BOUND('',#2215,.T.);
#878=FACE_BOUND('',#2217,.T.);
#879=FACE_BOUND('',#2220,.T.);
#880=FACE_BOUND('',#2223,.T.);
#881=FACE_BOUND('',#2229,.T.);
#882=FACE_BOUND('',#2232,.T.);
#883=FACE_BOUND('',#2234,.T.);
#884=FACE_BOUND('',#2235,.T.);
#885=FACE_BOUND('',#2237,.T.);
#886=FACE_BOUND('',#2238,.T.);
#887=FACE_BOUND('',#2242,.T.);
#888=FACE_BOUND('',#2244,.T.);
#889=FACE_BOUND('',#2248,.T.);
#890=FACE_BOUND('',#2250,.T.);
#891=FACE_BOUND('',#2255,.T.);
#892=FACE_BOUND('',#2258,.T.);
#893=FACE_BOUND('',#2271,.T.);
#894=FACE_BOUND('',#2272,.T.);
#895=FACE_BOUND('',#2275,.T.);
#896=FACE_BOUND('',#2278,.T.);
#897=FACE_BOUND('',#2281,.T.);
#898=FACE_BOUND('',#2284,.T.);
#899=FACE_BOUND('',#2294,.T.);
#900=FACE_BOUND('',#2295,.T.);
#901=FACE_BOUND('',#2296,.T.);
#902=FACE_BOUND('',#2297,.T.);
#903=FACE_BOUND('',#2304,.T.);
#904=FACE_BOUND('',#2305,.T.);
#905=FACE_BOUND('',#2306,.T.);
#906=FACE_BOUND('',#2307,.T.);
#907=FACE_BOUND('',#2316,.T.);
#908=FACE_BOUND('',#2319,.T.);
#909=FACE_BOUND('',#2324,.T.);
#910=FACE_BOUND('',#2329,.T.);
#911=FACE_BOUND('',#2357,.T.);
#912=FACE_BOUND('',#2360,.T.);
#913=FACE_BOUND('',#2363,.T.);
#914=FACE_BOUND('',#2366,.T.);
#915=FACE_BOUND('',#2369,.T.);
#916=FACE_BOUND('',#2386,.T.);
#917=FACE_BOUND('',#2387,.T.);
#918=FACE_BOUND('',#2388,.T.);
#919=FACE_BOUND('',#2389,.T.);
#920=FACE_BOUND('',#2390,.T.);
#921=FACE_BOUND('',#2391,.T.);
#922=FACE_BOUND('',#2392,.T.);
#923=FACE_BOUND('',#2393,.T.);
#924=FACE_BOUND('',#2394,.T.);
#925=FACE_BOUND('',#2395,.T.);
#926=FACE_BOUND('',#2397,.T.);
#927=FACE_BOUND('',#2398,.T.);
#928=FACE_BOUND('',#2399,.T.);
#929=FACE_BOUND('',#2400,.T.);
#930=FACE_BOUND('',#2401,.T.);
#931=FACE_BOUND('',#2402,.T.);
#932=FACE_BOUND('',#2403,.T.);
#933=FACE_BOUND('',#2404,.T.);
#934=FACE_BOUND('',#2405,.T.);
#935=FACE_BOUND('',#2406,.T.);
#936=FACE_BOUND('',#2421,.T.);
#937=FACE_BOUND('',#2422,.T.);
#938=FACE_BOUND('',#2423,.T.);
#939=FACE_BOUND('',#2424,.T.);
#940=FACE_BOUND('',#2425,.T.);
#941=FACE_BOUND('',#2427,.T.);
#942=FACE_BOUND('',#2428,.T.);
#943=FACE_BOUND('',#2429,.T.);
#944=FACE_BOUND('',#2430,.T.);
#945=FACE_BOUND('',#2431,.T.);
#946=FACE_BOUND('',#2437,.T.);
#947=FACE_BOUND('',#2438,.T.);
#948=FACE_BOUND('',#2440,.T.);
#949=FACE_BOUND('',#2441,.T.);
#950=FACE_BOUND('',#2448,.T.);
#951=FACE_BOUND('',#2449,.T.);
#952=FACE_BOUND('',#2450,.T.);
#953=FACE_BOUND('',#2451,.T.);
#954=FACE_BOUND('',#2455,.T.);
#955=FACE_BOUND('',#2457,.T.);
#956=FACE_BOUND('',#2463,.T.);
#957=FACE_BOUND('',#2470,.T.);
#958=FACE_BOUND('',#2473,.T.);
#959=FACE_BOUND('',#2479,.T.);
#960=FACE_BOUND('',#2486,.T.);
#961=FACE_BOUND('',#2489,.T.);
#962=FACE_BOUND('',#2497,.T.);
#963=FACE_BOUND('',#2500,.T.);
#964=FACE_BOUND('',#2503,.T.);
#965=FACE_BOUND('',#2504,.T.);
#966=FACE_BOUND('',#2514,.T.);
#967=FACE_BOUND('',#2517,.T.);
#968=FACE_BOUND('',#2519,.T.);
#969=FACE_BOUND('',#2535,.T.);
#970=FACE_BOUND('',#2536,.T.);
#971=FACE_BOUND('',#2537,.T.);
#972=FACE_BOUND('',#2538,.T.);
#973=FACE_BOUND('',#2581,.T.);
#974=FACE_BOUND('',#2589,.T.);
#975=FACE_BOUND('',#2592,.T.);
#976=FACE_BOUND('',#2597,.T.);
#977=FACE_BOUND('',#2602,.T.);
#978=FACE_BOUND('',#2627,.T.);
#979=FACE_BOUND('',#2630,.T.);
#980=FACE_BOUND('',#2633,.T.);
#981=FACE_BOUND('',#2636,.T.);
#982=FACE_BOUND('',#2639,.T.);
#983=FACE_BOUND('',#2655,.T.);
#984=FACE_BOUND('',#2661,.T.);
#985=FACE_BOUND('',#2663,.T.);
#986=FACE_BOUND('',#2668,.T.);
#987=FACE_BOUND('',#2672,.T.);
#988=FACE_BOUND('',#2675,.T.);
#989=FACE_BOUND('',#2679,.T.);
#990=FACE_BOUND('',#2681,.T.);
#991=FACE_BOUND('',#2685,.T.);
#992=FACE_BOUND('',#2687,.T.);
#993=FACE_BOUND('',#2697,.T.);
#994=FACE_BOUND('',#2699,.T.);
#995=FACE_BOUND('',#2703,.T.);
#996=FACE_BOUND('',#2704,.T.);
#997=FACE_BOUND('',#2705,.T.);
#998=FACE_BOUND('',#2709,.T.);
#999=FACE_BOUND('',#2710,.T.);
#1000=FACE_BOUND('',#2711,.T.);
#1001=FACE_BOUND('',#2713,.T.);
#1002=FACE_BOUND('',#2715,.T.);
#1003=FACE_BOUND('',#2718,.T.);
#1004=FACE_BOUND('',#2720,.T.);
#1005=FACE_BOUND('',#2723,.T.);
#1006=FACE_BOUND('',#2767,.T.);
#1007=FACE_BOUND('',#2769,.T.);
#1008=FACE_BOUND('',#2773,.T.);
#1009=FACE_BOUND('',#2779,.T.);
#1010=FACE_BOUND('',#2781,.T.);
#1011=FACE_BOUND('',#2785,.T.);
#1012=FACE_BOUND('',#2787,.T.);
#1013=FACE_BOUND('',#2797,.T.);
#1014=FACE_BOUND('',#2799,.T.);
#1015=FACE_BOUND('',#2803,.T.);
#1016=FACE_BOUND('',#2804,.T.);
#1017=FACE_BOUND('',#2805,.T.);
#1018=FACE_BOUND('',#2809,.T.);
#1019=FACE_BOUND('',#2810,.T.);
#1020=FACE_BOUND('',#2811,.T.);
#1021=FACE_BOUND('',#2813,.T.);
#1022=FACE_BOUND('',#2815,.T.);
#1023=FACE_BOUND('',#2818,.T.);
#1024=FACE_BOUND('',#2820,.T.);
#1025=FACE_BOUND('',#2823,.T.);
#1026=FACE_BOUND('',#2909,.T.);
#1027=FACE_BOUND('',#2925,.T.);
#1028=FACE_BOUND('',#2927,.T.);
#1029=FACE_BOUND('',#2931,.T.);
#1030=FACE_BOUND('',#2933,.T.);
#1031=FACE_BOUND('',#2937,.T.);
#1032=FACE_BOUND('',#2940,.T.);
#1033=FACE_BOUND('',#2945,.T.);
#1034=FACE_BOUND('',#2952,.T.);
#1035=FACE_BOUND('',#2954,.T.);
#1036=FACE_BOUND('',#2963,.T.);
#1037=PLANE('',#12882);
#1038=PLANE('',#12886);
#1039=PLANE('',#12890);
#1040=PLANE('',#12894);
#1041=PLANE('',#12898);
#1042=PLANE('',#12902);
#1043=PLANE('',#12906);
#1044=PLANE('',#12910);
#1045=PLANE('',#12914);
#1046=PLANE('',#12918);
#1047=PLANE('',#12922);
#1048=PLANE('',#12926);
#1049=PLANE('',#12930);
#1050=PLANE('',#12934);
#1051=PLANE('',#12935);
#1052=PLANE('',#12936);
#1053=PLANE('',#12937);
#1054=PLANE('',#12938);
#1055=PLANE('',#12939);
#1056=PLANE('',#12940);
#1057=PLANE('',#12942);
#1058=PLANE('',#12943);
#1059=PLANE('',#12944);
#1060=PLANE('',#12945);
#1061=PLANE('',#12946);
#1062=PLANE('',#12947);
#1063=PLANE('',#12949);
#1064=PLANE('',#12950);
#1065=PLANE('',#12951);
#1066=PLANE('',#12952);
#1067=PLANE('',#12953);
#1068=PLANE('',#12954);
#1069=PLANE('',#12983);
#1070=PLANE('',#12984);
#1071=PLANE('',#12985);
#1072=PLANE('',#12986);
#1073=PLANE('',#12987);
#1074=PLANE('',#12988);
#1075=PLANE('',#12989);
#1076=PLANE('',#12990);
#1077=PLANE('',#12991);
#1078=PLANE('',#12992);
#1079=PLANE('',#13000);
#1080=PLANE('',#13001);
#1081=PLANE('',#13015);
#1082=PLANE('',#13032);
#1083=PLANE('',#13035);
#1084=PLANE('',#13049);
#1085=PLANE('',#13065);
#1086=PLANE('',#13069);
#1087=PLANE('',#13074);
#1088=PLANE('',#13079);
#1089=PLANE('',#13088);
#1090=PLANE('',#13089);
#1091=PLANE('',#13090);
#1092=PLANE('',#13091);
#1093=PLANE('',#13092);
#1094=PLANE('',#13093);
#1095=PLANE('',#13101);
#1096=PLANE('',#13102);
#1097=PLANE('',#13107);
#1098=PLANE('',#13112);
#1099=PLANE('',#13121);
#1100=PLANE('',#13122);
#1101=PLANE('',#13123);
#1102=PLANE('',#13124);
#1103=PLANE('',#13125);
#1104=PLANE('',#13126);
#1105=PLANE('',#13134);
#1106=PLANE('',#13135);
#1107=PLANE('',#13143);
#1108=PLANE('',#13144);
#1109=PLANE('',#13155);
#1110=PLANE('',#13160);
#1111=PLANE('',#13162);
#1112=PLANE('',#13163);
#1113=PLANE('',#13164);
#1114=PLANE('',#13172);
#1115=PLANE('',#13173);
#1116=PLANE('',#13174);
#1117=PLANE('',#13175);
#1118=PLANE('',#13176);
#1119=PLANE('',#13177);
#1120=PLANE('',#13182);
#1121=PLANE('',#13187);
#1122=PLANE('',#13192);
#1123=PLANE('',#13197);
#1124=PLANE('',#13207);
#1125=PLANE('',#13208);
#1126=PLANE('',#13209);
#1127=PLANE('',#13210);
#1128=PLANE('',#13211);
#1129=PLANE('',#13212);
#1130=PLANE('',#13213);
#1131=PLANE('',#13214);
#1132=PLANE('',#13215);
#1133=PLANE('',#13216);
#1134=PLANE('',#13217);
#1135=PLANE('',#13218);
#1136=PLANE('',#13219);
#1137=PLANE('',#13220);
#1138=PLANE('',#13236);
#1139=PLANE('',#13239);
#1140=PLANE('',#13251);
#1141=PLANE('',#13260);
#1142=PLANE('',#13293);
#1143=PLANE('',#13298);
#1144=PLANE('',#13303);
#1145=PLANE('',#13308);
#1146=PLANE('',#13313);
#1147=PLANE('',#13318);
#1148=PLANE('',#13327);
#1149=PLANE('',#13331);
#1150=PLANE('',#13332);
#1151=PLANE('',#13334);
#1152=PLANE('',#13339);
#1153=PLANE('',#13342);
#1154=PLANE('',#13347);
#1155=PLANE('',#13387);
#1156=PLANE('',#13388);
#1157=PLANE('',#13389);
#1158=PLANE('',#13390);
#1159=PLANE('',#13391);
#1160=PLANE('',#13392);
#1161=PLANE('',#13409);
#1162=PLANE('',#13413);
#1163=PLANE('',#13417);
#1164=PLANE('',#13421);
#1165=PLANE('',#13425);
#1166=PLANE('',#13426);
#1167=PLANE('',#13439);
#1168=PLANE('',#13440);
#1169=PLANE('',#13441);
#1170=PLANE('',#13442);
#1171=PLANE('',#13443);
#1172=PLANE('',#13444);
#1173=PLANE('',#13445);
#1174=PLANE('',#13446);
#1175=PLANE('',#13454);
#1176=PLANE('',#13455);
#1177=PLANE('',#13469);
#1178=PLANE('',#13486);
#1179=PLANE('',#13489);
#1180=PLANE('',#13503);
#1181=PLANE('',#13519);
#1182=PLANE('',#13523);
#1183=PLANE('',#13528);
#1184=PLANE('',#13532);
#1185=PLANE('',#13536);
#1186=PLANE('',#13537);
#1187=PLANE('',#13538);
#1188=PLANE('',#13539);
#1189=PLANE('',#13540);
#1190=PLANE('',#13541);
#1191=PLANE('',#13543);
#1192=PLANE('',#13547);
#1193=PLANE('',#13549);
#1194=PLANE('',#13554);
#1195=PLANE('',#13558);
#1196=PLANE('',#13559);
#1197=PLANE('',#13560);
#1198=PLANE('',#13561);
#1199=PLANE('',#13562);
#1200=PLANE('',#13563);
#1201=PLANE('',#13566);
#1202=PLANE('',#13572);
#1203=PLANE('',#13578);
#1204=PLANE('',#13584);
#1205=PLANE('',#13590);
#1206=PLANE('',#13591);
#1207=PLANE('',#13592);
#1208=PLANE('',#13593);
#1209=PLANE('',#13594);
#1210=PLANE('',#13595);
#1211=PLANE('',#13596);
#1212=PLANE('',#13597);
#1213=PLANE('',#13598);
#1214=PLANE('',#13599);
#1215=PLANE('',#13600);
#1216=PLANE('',#13601);
#1217=PLANE('',#13602);
#1218=PLANE('',#13603);
#1219=PLANE('',#13605);
#1220=PLANE('',#13606);
#1221=PLANE('',#13607);
#1222=PLANE('',#13608);
#1223=PLANE('',#13609);
#1224=PLANE('',#13610);
#1225=PLANE('',#13611);
#1226=PLANE('',#13612);
#1227=PLANE('',#13613);
#1228=PLANE('',#13614);
#1229=PLANE('',#13616);
#1230=PLANE('',#13617);
#1231=PLANE('',#13618);
#1232=PLANE('',#13619);
#1233=PLANE('',#13620);
#1234=PLANE('',#13621);
#1235=PLANE('',#13622);
#1236=PLANE('',#13623);
#1237=PLANE('',#13624);
#1238=PLANE('',#13625);
#1239=PLANE('',#13630);
#1240=PLANE('',#13631);
#1241=PLANE('',#13632);
#1242=PLANE('',#13633);
#1243=PLANE('',#13634);
#1244=PLANE('',#13635);
#1245=PLANE('',#13636);
#1246=PLANE('',#13637);
#1247=PLANE('',#13638);
#1248=PLANE('',#13640);
#1249=PLANE('',#13648);
#1250=PLANE('',#13668);
#1251=PLANE('',#13671);
#1252=PLANE('',#13683);
#1253=PLANE('',#13692);
#1254=PLANE('',#13723);
#1255=PLANE('',#13728);
#1256=PLANE('',#13733);
#1257=PLANE('',#13739);
#1258=PLANE('',#13744);
#1259=PLANE('',#13753);
#1260=PLANE('',#13757);
#1261=PLANE('',#13758);
#1262=PLANE('',#13760);
#1263=PLANE('',#13765);
#1264=PLANE('',#13768);
#1265=PLANE('',#13773);
#1266=PLANE('',#13782);
#1267=PLANE('',#13783);
#1268=PLANE('',#13784);
#1269=PLANE('',#13785);
#1270=PLANE('',#13786);
#1271=PLANE('',#13787);
#1272=PLANE('',#13788);
#1273=PLANE('',#13789);
#1274=PLANE('',#13790);
#1275=PLANE('',#13792);
#1276=PLANE('',#13800);
#1277=PLANE('',#13810);
#1278=PLANE('',#13811);
#1279=PLANE('',#13814);
#1280=PLANE('',#13823);
#1281=PLANE('',#13826);
#1282=PLANE('',#13827);
#1283=PLANE('',#13832);
#1284=PLANE('',#13839);
#1285=PLANE('',#13840);
#1286=PLANE('',#13848);
#1287=PLANE('',#13849);
#1288=PLANE('',#13854);
#1289=PLANE('',#13855);
#1290=PLANE('',#13860);
#1291=PLANE('',#13861);
#1292=PLANE('',#13869);
#1293=PLANE('',#13870);
#1294=PLANE('',#13882);
#1295=PLANE('',#13883);
#1296=PLANE('',#13927);
#1297=PLANE('',#13928);
#1298=PLANE('',#13972);
#1299=PLANE('',#14018);
#1300=PLANE('',#14019);
#1301=PLANE('',#14022);
#1302=PLANE('',#14028);
#1303=PLANE('',#14031);
#1304=PLANE('',#14039);
#1305=PLANE('',#14040);
#1306=PLANE('',#14048);
#1307=PLANE('',#14049);
#1308=PLANE('',#14054);
#1309=PLANE('',#14055);
#1310=PLANE('',#14060);
#1311=PLANE('',#14061);
#1312=PLANE('',#14069);
#1313=PLANE('',#14070);
#1314=PLANE('',#14082);
#1315=PLANE('',#14083);
#1316=PLANE('',#14167);
#1317=PLANE('',#14168);
#1318=PLANE('',#14252);
#1319=PLANE('',#14334);
#1320=PLANE('',#14342);
#1321=PLANE('',#14350);
#1322=PLANE('',#14351);
#1323=PLANE('',#14352);
#1324=PLANE('',#14353);
#1325=PLANE('',#14354);
#1326=PLANE('',#14355);
#1327=PLANE('',#14356);
#1328=PLANE('',#14357);
#1329=PLANE('',#14358);
#1330=PLANE('',#14418);
#1331=PLANE('',#14419);
#1332=PLANE('',#14422);
#1333=PLANE('',#14428);
#1334=PLANE('',#14431);
#1335=PLANE('',#14437);
#1336=PLANE('',#14441);
#1337=PLANE('',#14446);
#1338=PLANE('',#14447);
#1339=PLANE('',#14449);
#1340=PLANE('',#14453);
#1341=PLANE('',#14460);
#1342=PLANE('',#14461);
#1343=PLANE('',#14463);
#1344=PLANE('',#14464);
#1345=PLANE('',#14465);
#1346=PLANE('',#14466);
#1347=PLANE('',#14467);
#1348=PLANE('',#14468);
#1349=PLANE('',#14469);
#1350=PLANE('',#14470);
#1351=PLANE('',#14478);
#1352=FACE_OUTER_BOUND('',#2056,.T.);
#1353=FACE_OUTER_BOUND('',#2057,.T.);
#1354=FACE_OUTER_BOUND('',#2058,.T.);
#1355=FACE_OUTER_BOUND('',#2059,.T.);
#1356=FACE_OUTER_BOUND('',#2060,.T.);
#1357=FACE_OUTER_BOUND('',#2061,.T.);
#1358=FACE_OUTER_BOUND('',#2062,.T.);
#1359=FACE_OUTER_BOUND('',#2063,.T.);
#1360=FACE_OUTER_BOUND('',#2064,.T.);
#1361=FACE_OUTER_BOUND('',#2065,.T.);
#1362=FACE_OUTER_BOUND('',#2066,.T.);
#1363=FACE_OUTER_BOUND('',#2067,.T.);
#1364=FACE_OUTER_BOUND('',#2068,.T.);
#1365=FACE_OUTER_BOUND('',#2069,.T.);
#1366=FACE_OUTER_BOUND('',#2070,.T.);
#1367=FACE_OUTER_BOUND('',#2071,.T.);
#1368=FACE_OUTER_BOUND('',#2072,.T.);
#1369=FACE_OUTER_BOUND('',#2073,.T.);
#1370=FACE_OUTER_BOUND('',#2074,.T.);
#1371=FACE_OUTER_BOUND('',#2075,.T.);
#1372=FACE_OUTER_BOUND('',#2076,.T.);
#1373=FACE_OUTER_BOUND('',#2077,.T.);
#1374=FACE_OUTER_BOUND('',#2078,.T.);
#1375=FACE_OUTER_BOUND('',#2079,.T.);
#1376=FACE_OUTER_BOUND('',#2080,.T.);
#1377=FACE_OUTER_BOUND('',#2081,.T.);
#1378=FACE_OUTER_BOUND('',#2082,.T.);
#1379=FACE_OUTER_BOUND('',#2083,.T.);
#1380=FACE_OUTER_BOUND('',#2084,.T.);
#1381=FACE_OUTER_BOUND('',#2085,.T.);
#1382=FACE_OUTER_BOUND('',#2086,.T.);
#1383=FACE_OUTER_BOUND('',#2087,.T.);
#1384=FACE_OUTER_BOUND('',#2088,.T.);
#1385=FACE_OUTER_BOUND('',#2103,.T.);
#1386=FACE_OUTER_BOUND('',#2104,.T.);
#1387=FACE_OUTER_BOUND('',#2105,.T.);
#1388=FACE_OUTER_BOUND('',#2106,.T.);
#1389=FACE_OUTER_BOUND('',#2107,.T.);
#1390=FACE_OUTER_BOUND('',#2108,.T.);
#1391=FACE_OUTER_BOUND('',#2109,.T.);
#1392=FACE_OUTER_BOUND('',#2110,.T.);
#1393=FACE_OUTER_BOUND('',#2111,.T.);
#1394=FACE_OUTER_BOUND('',#2112,.T.);
#1395=FACE_OUTER_BOUND('',#2113,.T.);
#1396=FACE_OUTER_BOUND('',#2114,.T.);
#1397=FACE_OUTER_BOUND('',#2115,.T.);
#1398=FACE_OUTER_BOUND('',#2116,.T.);
#1399=FACE_OUTER_BOUND('',#2117,.T.);
#1400=FACE_OUTER_BOUND('',#2118,.T.);
#1401=FACE_OUTER_BOUND('',#2119,.T.);
#1402=FACE_OUTER_BOUND('',#2120,.T.);
#1403=FACE_OUTER_BOUND('',#2121,.T.);
#1404=FACE_OUTER_BOUND('',#2122,.T.);
#1405=FACE_OUTER_BOUND('',#2123,.T.);
#1406=FACE_OUTER_BOUND('',#2124,.T.);
#1407=FACE_OUTER_BOUND('',#2125,.T.);
#1408=FACE_OUTER_BOUND('',#2128,.T.);
#1409=FACE_OUTER_BOUND('',#2131,.T.);
#1410=FACE_OUTER_BOUND('',#2132,.T.);
#1411=FACE_OUTER_BOUND('',#2133,.T.);
#1412=FACE_OUTER_BOUND('',#2139,.T.);
#1413=FACE_OUTER_BOUND('',#2140,.T.);
#1414=FACE_OUTER_BOUND('',#2146,.T.);
#1415=FACE_OUTER_BOUND('',#2147,.T.);
#1416=FACE_OUTER_BOUND('',#2148,.T.);
#1417=FACE_OUTER_BOUND('',#2153,.T.);
#1418=FACE_OUTER_BOUND('',#2154,.T.);
#1419=FACE_OUTER_BOUND('',#2155,.T.);
#1420=FACE_OUTER_BOUND('',#2157,.T.);
#1421=FACE_OUTER_BOUND('',#2159,.T.);
#1422=FACE_OUTER_BOUND('',#2160,.T.);
#1423=FACE_OUTER_BOUND('',#2161,.T.);
#1424=FACE_OUTER_BOUND('',#2162,.T.);
#1425=FACE_OUTER_BOUND('',#2163,.T.);
#1426=FACE_OUTER_BOUND('',#2165,.T.);
#1427=FACE_OUTER_BOUND('',#2166,.T.);
#1428=FACE_OUTER_BOUND('',#2167,.T.);
#1429=FACE_OUTER_BOUND('',#2168,.T.);
#1430=FACE_OUTER_BOUND('',#2169,.T.);
#1431=FACE_OUTER_BOUND('',#2170,.T.);
#1432=FACE_OUTER_BOUND('',#2172,.T.);
#1433=FACE_OUTER_BOUND('',#2173,.T.);
#1434=FACE_OUTER_BOUND('',#2175,.T.);
#1435=FACE_OUTER_BOUND('',#2176,.T.);
#1436=FACE_OUTER_BOUND('',#2177,.T.);
#1437=FACE_OUTER_BOUND('',#2178,.T.);
#1438=FACE_OUTER_BOUND('',#2179,.T.);
#1439=FACE_OUTER_BOUND('',#2181,.T.);
#1440=FACE_OUTER_BOUND('',#2182,.T.);
#1441=FACE_OUTER_BOUND('',#2183,.T.);
#1442=FACE_OUTER_BOUND('',#2184,.T.);
#1443=FACE_OUTER_BOUND('',#2185,.T.);
#1444=FACE_OUTER_BOUND('',#2186,.T.);
#1445=FACE_OUTER_BOUND('',#2188,.T.);
#1446=FACE_OUTER_BOUND('',#2189,.T.);
#1447=FACE_OUTER_BOUND('',#2191,.T.);
#1448=FACE_OUTER_BOUND('',#2192,.T.);
#1449=FACE_OUTER_BOUND('',#2194,.T.);
#1450=FACE_OUTER_BOUND('',#2195,.T.);
#1451=FACE_OUTER_BOUND('',#2197,.T.);
#1452=FACE_OUTER_BOUND('',#2198,.T.);
#1453=FACE_OUTER_BOUND('',#2199,.T.);
#1454=FACE_OUTER_BOUND('',#2200,.T.);
#1455=FACE_OUTER_BOUND('',#2201,.T.);
#1456=FACE_OUTER_BOUND('',#2203,.T.);
#1457=FACE_OUTER_BOUND('',#2204,.T.);
#1458=FACE_OUTER_BOUND('',#2206,.T.);
#1459=FACE_OUTER_BOUND('',#2209,.T.);
#1460=FACE_OUTER_BOUND('',#2212,.T.);
#1461=FACE_OUTER_BOUND('',#2213,.T.);
#1462=FACE_OUTER_BOUND('',#2214,.T.);
#1463=FACE_OUTER_BOUND('',#2216,.T.);
#1464=FACE_OUTER_BOUND('',#2218,.T.);
#1465=FACE_OUTER_BOUND('',#2219,.T.);
#1466=FACE_OUTER_BOUND('',#2221,.T.);
#1467=FACE_OUTER_BOUND('',#2222,.T.);
#1468=FACE_OUTER_BOUND('',#2224,.T.);
#1469=FACE_OUTER_BOUND('',#2225,.T.);
#1470=FACE_OUTER_BOUND('',#2226,.T.);
#1471=FACE_OUTER_BOUND('',#2227,.T.);
#1472=FACE_OUTER_BOUND('',#2228,.T.);
#1473=FACE_OUTER_BOUND('',#2230,.T.);
#1474=FACE_OUTER_BOUND('',#2231,.T.);
#1475=FACE_OUTER_BOUND('',#2233,.T.);
#1476=FACE_OUTER_BOUND('',#2236,.T.);
#1477=FACE_OUTER_BOUND('',#2239,.T.);
#1478=FACE_OUTER_BOUND('',#2240,.T.);
#1479=FACE_OUTER_BOUND('',#2241,.T.);
#1480=FACE_OUTER_BOUND('',#2243,.T.);
#1481=FACE_OUTER_BOUND('',#2245,.T.);
#1482=FACE_OUTER_BOUND('',#2246,.T.);
#1483=FACE_OUTER_BOUND('',#2247,.T.);
#1484=FACE_OUTER_BOUND('',#2249,.T.);
#1485=FACE_OUTER_BOUND('',#2251,.T.);
#1486=FACE_OUTER_BOUND('',#2252,.T.);
#1487=FACE_OUTER_BOUND('',#2253,.T.);
#1488=FACE_OUTER_BOUND('',#2254,.T.);
#1489=FACE_OUTER_BOUND('',#2256,.T.);
#1490=FACE_OUTER_BOUND('',#2257,.T.);
#1491=FACE_OUTER_BOUND('',#2259,.T.);
#1492=FACE_OUTER_BOUND('',#2260,.T.);
#1493=FACE_OUTER_BOUND('',#2261,.T.);
#1494=FACE_OUTER_BOUND('',#2262,.T.);
#1495=FACE_OUTER_BOUND('',#2263,.T.);
#1496=FACE_OUTER_BOUND('',#2264,.T.);
#1497=FACE_OUTER_BOUND('',#2265,.T.);
#1498=FACE_OUTER_BOUND('',#2266,.T.);
#1499=FACE_OUTER_BOUND('',#2267,.T.);
#1500=FACE_OUTER_BOUND('',#2268,.T.);
#1501=FACE_OUTER_BOUND('',#2269,.T.);
#1502=FACE_OUTER_BOUND('',#2270,.T.);
#1503=FACE_OUTER_BOUND('',#2273,.T.);
#1504=FACE_OUTER_BOUND('',#2274,.T.);
#1505=FACE_OUTER_BOUND('',#2276,.T.);
#1506=FACE_OUTER_BOUND('',#2277,.T.);
#1507=FACE_OUTER_BOUND('',#2279,.T.);
#1508=FACE_OUTER_BOUND('',#2280,.T.);
#1509=FACE_OUTER_BOUND('',#2282,.T.);
#1510=FACE_OUTER_BOUND('',#2283,.T.);
#1511=FACE_OUTER_BOUND('',#2285,.T.);
#1512=FACE_OUTER_BOUND('',#2286,.T.);
#1513=FACE_OUTER_BOUND('',#2287,.T.);
#1514=FACE_OUTER_BOUND('',#2288,.T.);
#1515=FACE_OUTER_BOUND('',#2289,.T.);
#1516=FACE_OUTER_BOUND('',#2290,.T.);
#1517=FACE_OUTER_BOUND('',#2291,.T.);
#1518=FACE_OUTER_BOUND('',#2292,.T.);
#1519=FACE_OUTER_BOUND('',#2293,.T.);
#1520=FACE_OUTER_BOUND('',#2298,.T.);
#1521=FACE_OUTER_BOUND('',#2299,.T.);
#1522=FACE_OUTER_BOUND('',#2300,.T.);
#1523=FACE_OUTER_BOUND('',#2301,.T.);
#1524=FACE_OUTER_BOUND('',#2302,.T.);
#1525=FACE_OUTER_BOUND('',#2303,.T.);
#1526=FACE_OUTER_BOUND('',#2308,.T.);
#1527=FACE_OUTER_BOUND('',#2309,.T.);
#1528=FACE_OUTER_BOUND('',#2310,.T.);
#1529=FACE_OUTER_BOUND('',#2311,.T.);
#1530=FACE_OUTER_BOUND('',#2312,.T.);
#1531=FACE_OUTER_BOUND('',#2313,.T.);
#1532=FACE_OUTER_BOUND('',#2314,.T.);
#1533=FACE_OUTER_BOUND('',#2315,.T.);
#1534=FACE_OUTER_BOUND('',#2317,.T.);
#1535=FACE_OUTER_BOUND('',#2318,.T.);
#1536=FACE_OUTER_BOUND('',#2320,.T.);
#1537=FACE_OUTER_BOUND('',#2321,.T.);
#1538=FACE_OUTER_BOUND('',#2322,.T.);
#1539=FACE_OUTER_BOUND('',#2323,.T.);
#1540=FACE_OUTER_BOUND('',#2325,.T.);
#1541=FACE_OUTER_BOUND('',#2326,.T.);
#1542=FACE_OUTER_BOUND('',#2327,.T.);
#1543=FACE_OUTER_BOUND('',#2328,.T.);
#1544=FACE_OUTER_BOUND('',#2330,.T.);
#1545=FACE_OUTER_BOUND('',#2331,.T.);
#1546=FACE_OUTER_BOUND('',#2332,.T.);
#1547=FACE_OUTER_BOUND('',#2333,.T.);
#1548=FACE_OUTER_BOUND('',#2334,.T.);
#1549=FACE_OUTER_BOUND('',#2335,.T.);
#1550=FACE_OUTER_BOUND('',#2336,.T.);
#1551=FACE_OUTER_BOUND('',#2337,.T.);
#1552=FACE_OUTER_BOUND('',#2338,.T.);
#1553=FACE_OUTER_BOUND('',#2339,.T.);
#1554=FACE_OUTER_BOUND('',#2340,.T.);
#1555=FACE_OUTER_BOUND('',#2341,.T.);
#1556=FACE_OUTER_BOUND('',#2342,.T.);
#1557=FACE_OUTER_BOUND('',#2343,.T.);
#1558=FACE_OUTER_BOUND('',#2344,.T.);
#1559=FACE_OUTER_BOUND('',#2345,.T.);
#1560=FACE_OUTER_BOUND('',#2346,.T.);
#1561=FACE_OUTER_BOUND('',#2347,.T.);
#1562=FACE_OUTER_BOUND('',#2348,.T.);
#1563=FACE_OUTER_BOUND('',#2349,.T.);
#1564=FACE_OUTER_BOUND('',#2350,.T.);
#1565=FACE_OUTER_BOUND('',#2351,.T.);
#1566=FACE_OUTER_BOUND('',#2352,.T.);
#1567=FACE_OUTER_BOUND('',#2353,.T.);
#1568=FACE_OUTER_BOUND('',#2354,.T.);
#1569=FACE_OUTER_BOUND('',#2355,.T.);
#1570=FACE_OUTER_BOUND('',#2356,.T.);
#1571=FACE_OUTER_BOUND('',#2358,.T.);
#1572=FACE_OUTER_BOUND('',#2359,.T.);
#1573=FACE_OUTER_BOUND('',#2361,.T.);
#1574=FACE_OUTER_BOUND('',#2362,.T.);
#1575=FACE_OUTER_BOUND('',#2364,.T.);
#1576=FACE_OUTER_BOUND('',#2365,.T.);
#1577=FACE_OUTER_BOUND('',#2367,.T.);
#1578=FACE_OUTER_BOUND('',#2368,.T.);
#1579=FACE_OUTER_BOUND('',#2370,.T.);
#1580=FACE_OUTER_BOUND('',#2371,.T.);
#1581=FACE_OUTER_BOUND('',#2372,.T.);
#1582=FACE_OUTER_BOUND('',#2373,.T.);
#1583=FACE_OUTER_BOUND('',#2374,.T.);
#1584=FACE_OUTER_BOUND('',#2375,.T.);
#1585=FACE_OUTER_BOUND('',#2376,.T.);
#1586=FACE_OUTER_BOUND('',#2377,.T.);
#1587=FACE_OUTER_BOUND('',#2378,.T.);
#1588=FACE_OUTER_BOUND('',#2379,.T.);
#1589=FACE_OUTER_BOUND('',#2380,.T.);
#1590=FACE_OUTER_BOUND('',#2381,.T.);
#1591=FACE_OUTER_BOUND('',#2382,.T.);
#1592=FACE_OUTER_BOUND('',#2383,.T.);
#1593=FACE_OUTER_BOUND('',#2384,.T.);
#1594=FACE_OUTER_BOUND('',#2385,.T.);
#1595=FACE_OUTER_BOUND('',#2396,.T.);
#1596=FACE_OUTER_BOUND('',#2407,.T.);
#1597=FACE_OUTER_BOUND('',#2408,.T.);
#1598=FACE_OUTER_BOUND('',#2409,.T.);
#1599=FACE_OUTER_BOUND('',#2410,.T.);
#1600=FACE_OUTER_BOUND('',#2411,.T.);
#1601=FACE_OUTER_BOUND('',#2412,.T.);
#1602=FACE_OUTER_BOUND('',#2413,.T.);
#1603=FACE_OUTER_BOUND('',#2414,.T.);
#1604=FACE_OUTER_BOUND('',#2415,.T.);
#1605=FACE_OUTER_BOUND('',#2416,.T.);
#1606=FACE_OUTER_BOUND('',#2417,.T.);
#1607=FACE_OUTER_BOUND('',#2418,.T.);
#1608=FACE_OUTER_BOUND('',#2419,.T.);
#1609=FACE_OUTER_BOUND('',#2420,.T.);
#1610=FACE_OUTER_BOUND('',#2426,.T.);
#1611=FACE_OUTER_BOUND('',#2432,.T.);
#1612=FACE_OUTER_BOUND('',#2433,.T.);
#1613=FACE_OUTER_BOUND('',#2434,.T.);
#1614=FACE_OUTER_BOUND('',#2435,.T.);
#1615=FACE_OUTER_BOUND('',#2436,.T.);
#1616=FACE_OUTER_BOUND('',#2439,.T.);
#1617=FACE_OUTER_BOUND('',#2442,.T.);
#1618=FACE_OUTER_BOUND('',#2443,.T.);
#1619=FACE_OUTER_BOUND('',#2444,.T.);
#1620=FACE_OUTER_BOUND('',#2445,.T.);
#1621=FACE_OUTER_BOUND('',#2446,.T.);
#1622=FACE_OUTER_BOUND('',#2447,.T.);
#1623=FACE_OUTER_BOUND('',#2452,.T.);
#1624=FACE_OUTER_BOUND('',#2453,.T.);
#1625=FACE_OUTER_BOUND('',#2454,.T.);
#1626=FACE_OUTER_BOUND('',#2456,.T.);
#1627=FACE_OUTER_BOUND('',#2458,.T.);
#1628=FACE_OUTER_BOUND('',#2459,.T.);
#1629=FACE_OUTER_BOUND('',#2460,.T.);
#1630=FACE_OUTER_BOUND('',#2461,.T.);
#1631=FACE_OUTER_BOUND('',#2462,.T.);
#1632=FACE_OUTER_BOUND('',#2464,.T.);
#1633=FACE_OUTER_BOUND('',#2465,.T.);
#1634=FACE_OUTER_BOUND('',#2466,.T.);
#1635=FACE_OUTER_BOUND('',#2467,.T.);
#1636=FACE_OUTER_BOUND('',#2468,.T.);
#1637=FACE_OUTER_BOUND('',#2469,.T.);
#1638=FACE_OUTER_BOUND('',#2471,.T.);
#1639=FACE_OUTER_BOUND('',#2472,.T.);
#1640=FACE_OUTER_BOUND('',#2474,.T.);
#1641=FACE_OUTER_BOUND('',#2475,.T.);
#1642=FACE_OUTER_BOUND('',#2476,.T.);
#1643=FACE_OUTER_BOUND('',#2477,.T.);
#1644=FACE_OUTER_BOUND('',#2478,.T.);
#1645=FACE_OUTER_BOUND('',#2480,.T.);
#1646=FACE_OUTER_BOUND('',#2481,.T.);
#1647=FACE_OUTER_BOUND('',#2482,.T.);
#1648=FACE_OUTER_BOUND('',#2483,.T.);
#1649=FACE_OUTER_BOUND('',#2484,.T.);
#1650=FACE_OUTER_BOUND('',#2485,.T.);
#1651=FACE_OUTER_BOUND('',#2487,.T.);
#1652=FACE_OUTER_BOUND('',#2488,.T.);
#1653=FACE_OUTER_BOUND('',#2490,.T.);
#1654=FACE_OUTER_BOUND('',#2491,.T.);
#1655=FACE_OUTER_BOUND('',#2492,.T.);
#1656=FACE_OUTER_BOUND('',#2493,.T.);
#1657=FACE_OUTER_BOUND('',#2494,.T.);
#1658=FACE_OUTER_BOUND('',#2495,.T.);
#1659=FACE_OUTER_BOUND('',#2496,.T.);
#1660=FACE_OUTER_BOUND('',#2498,.T.);
#1661=FACE_OUTER_BOUND('',#2499,.T.);
#1662=FACE_OUTER_BOUND('',#2501,.T.);
#1663=FACE_OUTER_BOUND('',#2502,.T.);
#1664=FACE_OUTER_BOUND('',#2505,.T.);
#1665=FACE_OUTER_BOUND('',#2506,.T.);
#1666=FACE_OUTER_BOUND('',#2507,.T.);
#1667=FACE_OUTER_BOUND('',#2508,.T.);
#1668=FACE_OUTER_BOUND('',#2509,.T.);
#1669=FACE_OUTER_BOUND('',#2510,.T.);
#1670=FACE_OUTER_BOUND('',#2511,.T.);
#1671=FACE_OUTER_BOUND('',#2512,.T.);
#1672=FACE_OUTER_BOUND('',#2513,.T.);
#1673=FACE_OUTER_BOUND('',#2515,.T.);
#1674=FACE_OUTER_BOUND('',#2516,.T.);
#1675=FACE_OUTER_BOUND('',#2518,.T.);
#1676=FACE_OUTER_BOUND('',#2520,.T.);
#1677=FACE_OUTER_BOUND('',#2521,.T.);
#1678=FACE_OUTER_BOUND('',#2522,.T.);
#1679=FACE_OUTER_BOUND('',#2523,.T.);
#1680=FACE_OUTER_BOUND('',#2524,.T.);
#1681=FACE_OUTER_BOUND('',#2525,.T.);
#1682=FACE_OUTER_BOUND('',#2526,.T.);
#1683=FACE_OUTER_BOUND('',#2527,.T.);
#1684=FACE_OUTER_BOUND('',#2528,.T.);
#1685=FACE_OUTER_BOUND('',#2529,.T.);
#1686=FACE_OUTER_BOUND('',#2530,.T.);
#1687=FACE_OUTER_BOUND('',#2531,.T.);
#1688=FACE_OUTER_BOUND('',#2532,.T.);
#1689=FACE_OUTER_BOUND('',#2533,.T.);
#1690=FACE_OUTER_BOUND('',#2534,.T.);
#1691=FACE_OUTER_BOUND('',#2539,.T.);
#1692=FACE_OUTER_BOUND('',#2540,.T.);
#1693=FACE_OUTER_BOUND('',#2541,.T.);
#1694=FACE_OUTER_BOUND('',#2542,.T.);
#1695=FACE_OUTER_BOUND('',#2543,.T.);
#1696=FACE_OUTER_BOUND('',#2544,.T.);
#1697=FACE_OUTER_BOUND('',#2545,.T.);
#1698=FACE_OUTER_BOUND('',#2546,.T.);
#1699=FACE_OUTER_BOUND('',#2547,.T.);
#1700=FACE_OUTER_BOUND('',#2548,.T.);
#1701=FACE_OUTER_BOUND('',#2549,.T.);
#1702=FACE_OUTER_BOUND('',#2550,.T.);
#1703=FACE_OUTER_BOUND('',#2551,.T.);
#1704=FACE_OUTER_BOUND('',#2552,.T.);
#1705=FACE_OUTER_BOUND('',#2553,.T.);
#1706=FACE_OUTER_BOUND('',#2554,.T.);
#1707=FACE_OUTER_BOUND('',#2555,.T.);
#1708=FACE_OUTER_BOUND('',#2556,.T.);
#1709=FACE_OUTER_BOUND('',#2557,.T.);
#1710=FACE_OUTER_BOUND('',#2558,.T.);
#1711=FACE_OUTER_BOUND('',#2559,.T.);
#1712=FACE_OUTER_BOUND('',#2560,.T.);
#1713=FACE_OUTER_BOUND('',#2561,.T.);
#1714=FACE_OUTER_BOUND('',#2562,.T.);
#1715=FACE_OUTER_BOUND('',#2563,.T.);
#1716=FACE_OUTER_BOUND('',#2564,.T.);
#1717=FACE_OUTER_BOUND('',#2565,.T.);
#1718=FACE_OUTER_BOUND('',#2566,.T.);
#1719=FACE_OUTER_BOUND('',#2567,.T.);
#1720=FACE_OUTER_BOUND('',#2568,.T.);
#1721=FACE_OUTER_BOUND('',#2569,.T.);
#1722=FACE_OUTER_BOUND('',#2570,.T.);
#1723=FACE_OUTER_BOUND('',#2571,.T.);
#1724=FACE_OUTER_BOUND('',#2572,.T.);
#1725=FACE_OUTER_BOUND('',#2573,.T.);
#1726=FACE_OUTER_BOUND('',#2574,.T.);
#1727=FACE_OUTER_BOUND('',#2575,.T.);
#1728=FACE_OUTER_BOUND('',#2576,.T.);
#1729=FACE_OUTER_BOUND('',#2577,.T.);
#1730=FACE_OUTER_BOUND('',#2578,.T.);
#1731=FACE_OUTER_BOUND('',#2579,.T.);
#1732=FACE_OUTER_BOUND('',#2580,.T.);
#1733=FACE_OUTER_BOUND('',#2582,.T.);
#1734=FACE_OUTER_BOUND('',#2583,.T.);
#1735=FACE_OUTER_BOUND('',#2584,.T.);
#1736=FACE_OUTER_BOUND('',#2585,.T.);
#1737=FACE_OUTER_BOUND('',#2586,.T.);
#1738=FACE_OUTER_BOUND('',#2587,.T.);
#1739=FACE_OUTER_BOUND('',#2588,.T.);
#1740=FACE_OUTER_BOUND('',#2590,.T.);
#1741=FACE_OUTER_BOUND('',#2591,.T.);
#1742=FACE_OUTER_BOUND('',#2593,.T.);
#1743=FACE_OUTER_BOUND('',#2594,.T.);
#1744=FACE_OUTER_BOUND('',#2595,.T.);
#1745=FACE_OUTER_BOUND('',#2596,.T.);
#1746=FACE_OUTER_BOUND('',#2598,.T.);
#1747=FACE_OUTER_BOUND('',#2599,.T.);
#1748=FACE_OUTER_BOUND('',#2600,.T.);
#1749=FACE_OUTER_BOUND('',#2601,.T.);
#1750=FACE_OUTER_BOUND('',#2603,.T.);
#1751=FACE_OUTER_BOUND('',#2604,.T.);
#1752=FACE_OUTER_BOUND('',#2605,.T.);
#1753=FACE_OUTER_BOUND('',#2606,.T.);
#1754=FACE_OUTER_BOUND('',#2607,.T.);
#1755=FACE_OUTER_BOUND('',#2608,.T.);
#1756=FACE_OUTER_BOUND('',#2609,.T.);
#1757=FACE_OUTER_BOUND('',#2610,.T.);
#1758=FACE_OUTER_BOUND('',#2611,.T.);
#1759=FACE_OUTER_BOUND('',#2612,.T.);
#1760=FACE_OUTER_BOUND('',#2613,.T.);
#1761=FACE_OUTER_BOUND('',#2614,.T.);
#1762=FACE_OUTER_BOUND('',#2615,.T.);
#1763=FACE_OUTER_BOUND('',#2616,.T.);
#1764=FACE_OUTER_BOUND('',#2617,.T.);
#1765=FACE_OUTER_BOUND('',#2618,.T.);
#1766=FACE_OUTER_BOUND('',#2619,.T.);
#1767=FACE_OUTER_BOUND('',#2620,.T.);
#1768=FACE_OUTER_BOUND('',#2621,.T.);
#1769=FACE_OUTER_BOUND('',#2622,.T.);
#1770=FACE_OUTER_BOUND('',#2623,.T.);
#1771=FACE_OUTER_BOUND('',#2624,.T.);
#1772=FACE_OUTER_BOUND('',#2625,.T.);
#1773=FACE_OUTER_BOUND('',#2626,.T.);
#1774=FACE_OUTER_BOUND('',#2628,.T.);
#1775=FACE_OUTER_BOUND('',#2629,.T.);
#1776=FACE_OUTER_BOUND('',#2631,.T.);
#1777=FACE_OUTER_BOUND('',#2632,.T.);
#1778=FACE_OUTER_BOUND('',#2634,.T.);
#1779=FACE_OUTER_BOUND('',#2635,.T.);
#1780=FACE_OUTER_BOUND('',#2637,.T.);
#1781=FACE_OUTER_BOUND('',#2638,.T.);
#1782=FACE_OUTER_BOUND('',#2640,.T.);
#1783=FACE_OUTER_BOUND('',#2641,.T.);
#1784=FACE_OUTER_BOUND('',#2642,.T.);
#1785=FACE_OUTER_BOUND('',#2643,.T.);
#1786=FACE_OUTER_BOUND('',#2644,.T.);
#1787=FACE_OUTER_BOUND('',#2645,.T.);
#1788=FACE_OUTER_BOUND('',#2646,.T.);
#1789=FACE_OUTER_BOUND('',#2647,.T.);
#1790=FACE_OUTER_BOUND('',#2648,.T.);
#1791=FACE_OUTER_BOUND('',#2649,.T.);
#1792=FACE_OUTER_BOUND('',#2650,.T.);
#1793=FACE_OUTER_BOUND('',#2651,.T.);
#1794=FACE_OUTER_BOUND('',#2652,.T.);
#1795=FACE_OUTER_BOUND('',#2653,.T.);
#1796=FACE_OUTER_BOUND('',#2654,.T.);
#1797=FACE_OUTER_BOUND('',#2656,.T.);
#1798=FACE_OUTER_BOUND('',#2657,.T.);
#1799=FACE_OUTER_BOUND('',#2658,.T.);
#1800=FACE_OUTER_BOUND('',#2659,.T.);
#1801=FACE_OUTER_BOUND('',#2660,.T.);
#1802=FACE_OUTER_BOUND('',#2662,.T.);
#1803=FACE_OUTER_BOUND('',#2664,.T.);
#1804=FACE_OUTER_BOUND('',#2665,.T.);
#1805=FACE_OUTER_BOUND('',#2666,.T.);
#1806=FACE_OUTER_BOUND('',#2667,.T.);
#1807=FACE_OUTER_BOUND('',#2669,.T.);
#1808=FACE_OUTER_BOUND('',#2670,.T.);
#1809=FACE_OUTER_BOUND('',#2671,.T.);
#1810=FACE_OUTER_BOUND('',#2673,.T.);
#1811=FACE_OUTER_BOUND('',#2674,.T.);
#1812=FACE_OUTER_BOUND('',#2676,.T.);
#1813=FACE_OUTER_BOUND('',#2677,.T.);
#1814=FACE_OUTER_BOUND('',#2678,.T.);
#1815=FACE_OUTER_BOUND('',#2680,.T.);
#1816=FACE_OUTER_BOUND('',#2682,.T.);
#1817=FACE_OUTER_BOUND('',#2683,.T.);
#1818=FACE_OUTER_BOUND('',#2684,.T.);
#1819=FACE_OUTER_BOUND('',#2686,.T.);
#1820=FACE_OUTER_BOUND('',#2688,.T.);
#1821=FACE_OUTER_BOUND('',#2689,.T.);
#1822=FACE_OUTER_BOUND('',#2690,.T.);
#1823=FACE_OUTER_BOUND('',#2691,.T.);
#1824=FACE_OUTER_BOUND('',#2692,.T.);
#1825=FACE_OUTER_BOUND('',#2693,.T.);
#1826=FACE_OUTER_BOUND('',#2694,.T.);
#1827=FACE_OUTER_BOUND('',#2695,.T.);
#1828=FACE_OUTER_BOUND('',#2696,.T.);
#1829=FACE_OUTER_BOUND('',#2698,.T.);
#1830=FACE_OUTER_BOUND('',#2700,.T.);
#1831=FACE_OUTER_BOUND('',#2701,.T.);
#1832=FACE_OUTER_BOUND('',#2702,.T.);
#1833=FACE_OUTER_BOUND('',#2706,.T.);
#1834=FACE_OUTER_BOUND('',#2707,.T.);
#1835=FACE_OUTER_BOUND('',#2708,.T.);
#1836=FACE_OUTER_BOUND('',#2712,.T.);
#1837=FACE_OUTER_BOUND('',#2714,.T.);
#1838=FACE_OUTER_BOUND('',#2716,.T.);
#1839=FACE_OUTER_BOUND('',#2717,.T.);
#1840=FACE_OUTER_BOUND('',#2719,.T.);
#1841=FACE_OUTER_BOUND('',#2721,.T.);
#1842=FACE_OUTER_BOUND('',#2722,.T.);
#1843=FACE_OUTER_BOUND('',#2724,.T.);
#1844=FACE_OUTER_BOUND('',#2725,.T.);
#1845=FACE_OUTER_BOUND('',#2726,.T.);
#1846=FACE_OUTER_BOUND('',#2727,.T.);
#1847=FACE_OUTER_BOUND('',#2728,.T.);
#1848=FACE_OUTER_BOUND('',#2729,.T.);
#1849=FACE_OUTER_BOUND('',#2730,.T.);
#1850=FACE_OUTER_BOUND('',#2731,.T.);
#1851=FACE_OUTER_BOUND('',#2732,.T.);
#1852=FACE_OUTER_BOUND('',#2733,.T.);
#1853=FACE_OUTER_BOUND('',#2734,.T.);
#1854=FACE_OUTER_BOUND('',#2735,.T.);
#1855=FACE_OUTER_BOUND('',#2736,.T.);
#1856=FACE_OUTER_BOUND('',#2737,.T.);
#1857=FACE_OUTER_BOUND('',#2738,.T.);
#1858=FACE_OUTER_BOUND('',#2739,.T.);
#1859=FACE_OUTER_BOUND('',#2740,.T.);
#1860=FACE_OUTER_BOUND('',#2741,.T.);
#1861=FACE_OUTER_BOUND('',#2742,.T.);
#1862=FACE_OUTER_BOUND('',#2743,.T.);
#1863=FACE_OUTER_BOUND('',#2744,.T.);
#1864=FACE_OUTER_BOUND('',#2745,.T.);
#1865=FACE_OUTER_BOUND('',#2746,.T.);
#1866=FACE_OUTER_BOUND('',#2747,.T.);
#1867=FACE_OUTER_BOUND('',#2748,.T.);
#1868=FACE_OUTER_BOUND('',#2749,.T.);
#1869=FACE_OUTER_BOUND('',#2750,.T.);
#1870=FACE_OUTER_BOUND('',#2751,.T.);
#1871=FACE_OUTER_BOUND('',#2752,.T.);
#1872=FACE_OUTER_BOUND('',#2753,.T.);
#1873=FACE_OUTER_BOUND('',#2754,.T.);
#1874=FACE_OUTER_BOUND('',#2755,.T.);
#1875=FACE_OUTER_BOUND('',#2756,.T.);
#1876=FACE_OUTER_BOUND('',#2757,.T.);
#1877=FACE_OUTER_BOUND('',#2758,.T.);
#1878=FACE_OUTER_BOUND('',#2759,.T.);
#1879=FACE_OUTER_BOUND('',#2760,.T.);
#1880=FACE_OUTER_BOUND('',#2761,.T.);
#1881=FACE_OUTER_BOUND('',#2762,.T.);
#1882=FACE_OUTER_BOUND('',#2763,.T.);
#1883=FACE_OUTER_BOUND('',#2764,.T.);
#1884=FACE_OUTER_BOUND('',#2765,.T.);
#1885=FACE_OUTER_BOUND('',#2766,.T.);
#1886=FACE_OUTER_BOUND('',#2768,.T.);
#1887=FACE_OUTER_BOUND('',#2770,.T.);
#1888=FACE_OUTER_BOUND('',#2771,.T.);
#1889=FACE_OUTER_BOUND('',#2772,.T.);
#1890=FACE_OUTER_BOUND('',#2774,.T.);
#1891=FACE_OUTER_BOUND('',#2775,.T.);
#1892=FACE_OUTER_BOUND('',#2776,.T.);
#1893=FACE_OUTER_BOUND('',#2777,.T.);
#1894=FACE_OUTER_BOUND('',#2778,.T.);
#1895=FACE_OUTER_BOUND('',#2780,.T.);
#1896=FACE_OUTER_BOUND('',#2782,.T.);
#1897=FACE_OUTER_BOUND('',#2783,.T.);
#1898=FACE_OUTER_BOUND('',#2784,.T.);
#1899=FACE_OUTER_BOUND('',#2786,.T.);
#1900=FACE_OUTER_BOUND('',#2788,.T.);
#1901=FACE_OUTER_BOUND('',#2789,.T.);
#1902=FACE_OUTER_BOUND('',#2790,.T.);
#1903=FACE_OUTER_BOUND('',#2791,.T.);
#1904=FACE_OUTER_BOUND('',#2792,.T.);
#1905=FACE_OUTER_BOUND('',#2793,.T.);
#1906=FACE_OUTER_BOUND('',#2794,.T.);
#1907=FACE_OUTER_BOUND('',#2795,.T.);
#1908=FACE_OUTER_BOUND('',#2796,.T.);
#1909=FACE_OUTER_BOUND('',#2798,.T.);
#1910=FACE_OUTER_BOUND('',#2800,.T.);
#1911=FACE_OUTER_BOUND('',#2801,.T.);
#1912=FACE_OUTER_BOUND('',#2802,.T.);
#1913=FACE_OUTER_BOUND('',#2806,.T.);
#1914=FACE_OUTER_BOUND('',#2807,.T.);
#1915=FACE_OUTER_BOUND('',#2808,.T.);
#1916=FACE_OUTER_BOUND('',#2812,.T.);
#1917=FACE_OUTER_BOUND('',#2814,.T.);
#1918=FACE_OUTER_BOUND('',#2816,.T.);
#1919=FACE_OUTER_BOUND('',#2817,.T.);
#1920=FACE_OUTER_BOUND('',#2819,.T.);
#1921=FACE_OUTER_BOUND('',#2821,.T.);
#1922=FACE_OUTER_BOUND('',#2822,.T.);
#1923=FACE_OUTER_BOUND('',#2824,.T.);
#1924=FACE_OUTER_BOUND('',#2825,.T.);
#1925=FACE_OUTER_BOUND('',#2826,.T.);
#1926=FACE_OUTER_BOUND('',#2827,.T.);
#1927=FACE_OUTER_BOUND('',#2828,.T.);
#1928=FACE_OUTER_BOUND('',#2829,.T.);
#1929=FACE_OUTER_BOUND('',#2830,.T.);
#1930=FACE_OUTER_BOUND('',#2831,.T.);
#1931=FACE_OUTER_BOUND('',#2832,.T.);
#1932=FACE_OUTER_BOUND('',#2833,.T.);
#1933=FACE_OUTER_BOUND('',#2834,.T.);
#1934=FACE_OUTER_BOUND('',#2835,.T.);
#1935=FACE_OUTER_BOUND('',#2836,.T.);
#1936=FACE_OUTER_BOUND('',#2837,.T.);
#1937=FACE_OUTER_BOUND('',#2838,.T.);
#1938=FACE_OUTER_BOUND('',#2839,.T.);
#1939=FACE_OUTER_BOUND('',#2840,.T.);
#1940=FACE_OUTER_BOUND('',#2841,.T.);
#1941=FACE_OUTER_BOUND('',#2842,.T.);
#1942=FACE_OUTER_BOUND('',#2843,.T.);
#1943=FACE_OUTER_BOUND('',#2844,.T.);
#1944=FACE_OUTER_BOUND('',#2845,.T.);
#1945=FACE_OUTER_BOUND('',#2846,.T.);
#1946=FACE_OUTER_BOUND('',#2847,.T.);
#1947=FACE_OUTER_BOUND('',#2848,.T.);
#1948=FACE_OUTER_BOUND('',#2849,.T.);
#1949=FACE_OUTER_BOUND('',#2850,.T.);
#1950=FACE_OUTER_BOUND('',#2851,.T.);
#1951=FACE_OUTER_BOUND('',#2852,.T.);
#1952=FACE_OUTER_BOUND('',#2853,.T.);
#1953=FACE_OUTER_BOUND('',#2854,.T.);
#1954=FACE_OUTER_BOUND('',#2855,.T.);
#1955=FACE_OUTER_BOUND('',#2856,.T.);
#1956=FACE_OUTER_BOUND('',#2857,.T.);
#1957=FACE_OUTER_BOUND('',#2858,.T.);
#1958=FACE_OUTER_BOUND('',#2859,.T.);
#1959=FACE_OUTER_BOUND('',#2860,.T.);
#1960=FACE_OUTER_BOUND('',#2861,.T.);
#1961=FACE_OUTER_BOUND('',#2862,.T.);
#1962=FACE_OUTER_BOUND('',#2863,.T.);
#1963=FACE_OUTER_BOUND('',#2864,.T.);
#1964=FACE_OUTER_BOUND('',#2865,.T.);
#1965=FACE_OUTER_BOUND('',#2866,.T.);
#1966=FACE_OUTER_BOUND('',#2867,.T.);
#1967=FACE_OUTER_BOUND('',#2868,.T.);
#1968=FACE_OUTER_BOUND('',#2869,.T.);
#1969=FACE_OUTER_BOUND('',#2870,.T.);
#1970=FACE_OUTER_BOUND('',#2871,.T.);
#1971=FACE_OUTER_BOUND('',#2872,.T.);
#1972=FACE_OUTER_BOUND('',#2873,.T.);
#1973=FACE_OUTER_BOUND('',#2874,.T.);
#1974=FACE_OUTER_BOUND('',#2875,.T.);
#1975=FACE_OUTER_BOUND('',#2876,.T.);
#1976=FACE_OUTER_BOUND('',#2877,.T.);
#1977=FACE_OUTER_BOUND('',#2878,.T.);
#1978=FACE_OUTER_BOUND('',#2879,.T.);
#1979=FACE_OUTER_BOUND('',#2880,.T.);
#1980=FACE_OUTER_BOUND('',#2881,.T.);
#1981=FACE_OUTER_BOUND('',#2882,.T.);
#1982=FACE_OUTER_BOUND('',#2883,.T.);
#1983=FACE_OUTER_BOUND('',#2884,.T.);
#1984=FACE_OUTER_BOUND('',#2885,.T.);
#1985=FACE_OUTER_BOUND('',#2886,.T.);
#1986=FACE_OUTER_BOUND('',#2887,.T.);
#1987=FACE_OUTER_BOUND('',#2888,.T.);
#1988=FACE_OUTER_BOUND('',#2889,.T.);
#1989=FACE_OUTER_BOUND('',#2890,.T.);
#1990=FACE_OUTER_BOUND('',#2891,.T.);
#1991=FACE_OUTER_BOUND('',#2892,.T.);
#1992=FACE_OUTER_BOUND('',#2893,.T.);
#1993=FACE_OUTER_BOUND('',#2894,.T.);
#1994=FACE_OUTER_BOUND('',#2895,.T.);
#1995=FACE_OUTER_BOUND('',#2896,.T.);
#1996=FACE_OUTER_BOUND('',#2897,.T.);
#1997=FACE_OUTER_BOUND('',#2898,.T.);
#1998=FACE_OUTER_BOUND('',#2899,.T.);
#1999=FACE_OUTER_BOUND('',#2900,.T.);
#2000=FACE_OUTER_BOUND('',#2901,.T.);
#2001=FACE_OUTER_BOUND('',#2902,.T.);
#2002=FACE_OUTER_BOUND('',#2903,.T.);
#2003=FACE_OUTER_BOUND('',#2904,.T.);
#2004=FACE_OUTER_BOUND('',#2905,.T.);
#2005=FACE_OUTER_BOUND('',#2906,.T.);
#2006=FACE_OUTER_BOUND('',#2907,.T.);
#2007=FACE_OUTER_BOUND('',#2908,.T.);
#2008=FACE_OUTER_BOUND('',#2910,.T.);
#2009=FACE_OUTER_BOUND('',#2911,.T.);
#2010=FACE_OUTER_BOUND('',#2912,.T.);
#2011=FACE_OUTER_BOUND('',#2913,.T.);
#2012=FACE_OUTER_BOUND('',#2914,.T.);
#2013=FACE_OUTER_BOUND('',#2915,.T.);
#2014=FACE_OUTER_BOUND('',#2916,.T.);
#2015=FACE_OUTER_BOUND('',#2917,.T.);
#2016=FACE_OUTER_BOUND('',#2918,.T.);
#2017=FACE_OUTER_BOUND('',#2919,.T.);
#2018=FACE_OUTER_BOUND('',#2920,.T.);
#2019=FACE_OUTER_BOUND('',#2921,.T.);
#2020=FACE_OUTER_BOUND('',#2922,.T.);
#2021=FACE_OUTER_BOUND('',#2923,.T.);
#2022=FACE_OUTER_BOUND('',#2924,.T.);
#2023=FACE_OUTER_BOUND('',#2926,.T.);
#2024=FACE_OUTER_BOUND('',#2928,.T.);
#2025=FACE_OUTER_BOUND('',#2929,.T.);
#2026=FACE_OUTER_BOUND('',#2930,.T.);
#2027=FACE_OUTER_BOUND('',#2932,.T.);
#2028=FACE_OUTER_BOUND('',#2934,.T.);
#2029=FACE_OUTER_BOUND('',#2935,.T.);
#2030=FACE_OUTER_BOUND('',#2936,.T.);
#2031=FACE_OUTER_BOUND('',#2938,.T.);
#2032=FACE_OUTER_BOUND('',#2939,.T.);
#2033=FACE_OUTER_BOUND('',#2941,.T.);
#2034=FACE_OUTER_BOUND('',#2942,.T.);
#2035=FACE_OUTER_BOUND('',#2943,.T.);
#2036=FACE_OUTER_BOUND('',#2944,.T.);
#2037=FACE_OUTER_BOUND('',#2946,.T.);
#2038=FACE_OUTER_BOUND('',#2947,.T.);
#2039=FACE_OUTER_BOUND('',#2948,.T.);
#2040=FACE_OUTER_BOUND('',#2949,.T.);
#2041=FACE_OUTER_BOUND('',#2950,.T.);
#2042=FACE_OUTER_BOUND('',#2951,.T.);
#2043=FACE_OUTER_BOUND('',#2953,.T.);
#2044=FACE_OUTER_BOUND('',#2955,.T.);
#2045=FACE_OUTER_BOUND('',#2956,.T.);
#2046=FACE_OUTER_BOUND('',#2957,.T.);
#2047=FACE_OUTER_BOUND('',#2958,.T.);
#2048=FACE_OUTER_BOUND('',#2959,.T.);
#2049=FACE_OUTER_BOUND('',#2960,.T.);
#2050=FACE_OUTER_BOUND('',#2961,.T.);
#2051=FACE_OUTER_BOUND('',#2962,.T.);
#2052=FACE_OUTER_BOUND('',#2964,.T.);
#2053=FACE_OUTER_BOUND('',#2965,.T.);
#2054=FACE_OUTER_BOUND('',#2966,.T.);
#2055=FACE_OUTER_BOUND('',#2967,.T.);
#2056=EDGE_LOOP('',(#7938,#7939,#7940,#7941));
#2057=EDGE_LOOP('',(#7942));
#2058=EDGE_LOOP('',(#7943,#7944,#7945,#7946));
#2059=EDGE_LOOP('',(#7947));
#2060=EDGE_LOOP('',(#7948,#7949,#7950,#7951));
#2061=EDGE_LOOP('',(#7952));
#2062=EDGE_LOOP('',(#7953,#7954,#7955,#7956));
#2063=EDGE_LOOP('',(#7957));
#2064=EDGE_LOOP('',(#7958,#7959,#7960,#7961));
#2065=EDGE_LOOP('',(#7962));
#2066=EDGE_LOOP('',(#7963,#7964,#7965,#7966));
#2067=EDGE_LOOP('',(#7967));
#2068=EDGE_LOOP('',(#7968,#7969,#7970,#7971));
#2069=EDGE_LOOP('',(#7972));
#2070=EDGE_LOOP('',(#7973,#7974,#7975,#7976));
#2071=EDGE_LOOP('',(#7977));
#2072=EDGE_LOOP('',(#7978,#7979,#7980,#7981));
#2073=EDGE_LOOP('',(#7982));
#2074=EDGE_LOOP('',(#7983,#7984,#7985,#7986));
#2075=EDGE_LOOP('',(#7987));
#2076=EDGE_LOOP('',(#7988,#7989,#7990,#7991));
#2077=EDGE_LOOP('',(#7992));
#2078=EDGE_LOOP('',(#7993,#7994,#7995,#7996));
#2079=EDGE_LOOP('',(#7997));
#2080=EDGE_LOOP('',(#7998,#7999,#8000,#8001));
#2081=EDGE_LOOP('',(#8002));
#2082=EDGE_LOOP('',(#8003,#8004,#8005,#8006));
#2083=EDGE_LOOP('',(#8007));
#2084=EDGE_LOOP('',(#8008,#8009,#8010,#8011));
#2085=EDGE_LOOP('',(#8012,#8013,#8014,#8015));
#2086=EDGE_LOOP('',(#8016,#8017,#8018,#8019));
#2087=EDGE_LOOP('',(#8020,#8021,#8022,#8023));
#2088=EDGE_LOOP('',(#8024,#8025,#8026,#8027));
#2089=EDGE_LOOP('',(#8028));
#2090=EDGE_LOOP('',(#8029));
#2091=EDGE_LOOP('',(#8030));
#2092=EDGE_LOOP('',(#8031));
#2093=EDGE_LOOP('',(#8032));
#2094=EDGE_LOOP('',(#8033));
#2095=EDGE_LOOP('',(#8034));
#2096=EDGE_LOOP('',(#8035));
#2097=EDGE_LOOP('',(#8036));
#2098=EDGE_LOOP('',(#8037));
#2099=EDGE_LOOP('',(#8038));
#2100=EDGE_LOOP('',(#8039));
#2101=EDGE_LOOP('',(#8040));
#2102=EDGE_LOOP('',(#8041));
#2103=EDGE_LOOP('',(#8042,#8043,#8044,#8045));
#2104=EDGE_LOOP('',(#8046,#8047,#8048,#8049));
#2105=EDGE_LOOP('',(#8050,#8051,#8052,#8053));
#2106=EDGE_LOOP('',(#8054,#8055,#8056,#8057));
#2107=EDGE_LOOP('',(#8058,#8059,#8060,#8061));
#2108=EDGE_LOOP('',(#8062,#8063,#8064,#8065));
#2109=EDGE_LOOP('',(#8066,#8067,#8068,#8069));
#2110=EDGE_LOOP('',(#8070,#8071,#8072,#8073));
#2111=EDGE_LOOP('',(#8074,#8075,#8076,#8077));
#2112=EDGE_LOOP('',(#8078,#8079,#8080,#8081));
#2113=EDGE_LOOP('',(#8082,#8083,#8084,#8085));
#2114=EDGE_LOOP('',(#8086,#8087,#8088,#8089));
#2115=EDGE_LOOP('',(#8090,#8091,#8092,#8093));
#2116=EDGE_LOOP('',(#8094,#8095,#8096,#8097));
#2117=EDGE_LOOP('',(#8098,#8099,#8100,#8101));
#2118=EDGE_LOOP('',(#8102,#8103,#8104,#8105));
#2119=EDGE_LOOP('',(#8106,#8107,#8108,#8109));
#2120=EDGE_LOOP('',(#8110,#8111,#8112,#8113));
#2121=EDGE_LOOP('',(#8114,#8115,#8116,#8117));
#2122=EDGE_LOOP('',(#8118,#8119,#8120,#8121));
#2123=EDGE_LOOP('',(#8122,#8123,#8124,#8125));
#2124=EDGE_LOOP('',(#8126,#8127,#8128,#8129));
#2125=EDGE_LOOP('',(#8130,#8131,#8132,#8133));
#2126=EDGE_LOOP('',(#8134));
#2127=EDGE_LOOP('',(#8135));
#2128=EDGE_LOOP('',(#8136,#8137,#8138,#8139));
#2129=EDGE_LOOP('',(#8140));
#2130=EDGE_LOOP('',(#8141));
#2131=EDGE_LOOP('',(#8142,#8143,#8144,#8145));
#2132=EDGE_LOOP('',(#8146,#8147,#8148,#8149));
#2133=EDGE_LOOP('',(#8150,#8151,#8152,#8153,#8154,#8155,#8156,#8157));
#2134=EDGE_LOOP('',(#8158));
#2135=EDGE_LOOP('',(#8159));
#2136=EDGE_LOOP('',(#8160));
#2137=EDGE_LOOP('',(#8161));
#2138=EDGE_LOOP('',(#8162));
#2139=EDGE_LOOP('',(#8163,#8164,#8165,#8166));
#2140=EDGE_LOOP('',(#8167,#8168,#8169,#8170,#8171,#8172,#8173,#8174));
#2141=EDGE_LOOP('',(#8175));
#2142=EDGE_LOOP('',(#8176));
#2143=EDGE_LOOP('',(#8177));
#2144=EDGE_LOOP('',(#8178));
#2145=EDGE_LOOP('',(#8179));
#2146=EDGE_LOOP('',(#8180,#8181,#8182,#8183));
#2147=EDGE_LOOP('',(#8184,#8185,#8186,#8187));
#2148=EDGE_LOOP('',(#8188,#8189,#8190,#8191));
#2149=EDGE_LOOP('',(#8192));
#2150=EDGE_LOOP('',(#8193));
#2151=EDGE_LOOP('',(#8194));
#2152=EDGE_LOOP('',(#8195));
#2153=EDGE_LOOP('',(#8196,#8197,#8198,#8199));
#2154=EDGE_LOOP('',(#8200,#8201,#8202,#8203));
#2155=EDGE_LOOP('',(#8204));
#2156=EDGE_LOOP('',(#8205));
#2157=EDGE_LOOP('',(#8206));
#2158=EDGE_LOOP('',(#8207));
#2159=EDGE_LOOP('',(#8208,#8209,#8210,#8211));
#2160=EDGE_LOOP('',(#8212,#8213,#8214,#8215));
#2161=EDGE_LOOP('',(#8216,#8217,#8218,#8219));
#2162=EDGE_LOOP('',(#8220,#8221,#8222,#8223));
#2163=EDGE_LOOP('',(#8224,#8225,#8226,#8227,#8228,#8229,#8230,#8231));
#2164=EDGE_LOOP('',(#8232));
#2165=EDGE_LOOP('',(#8233,#8234,#8235,#8236));
#2166=EDGE_LOOP('',(#8237,#8238,#8239,#8240));
#2167=EDGE_LOOP('',(#8241,#8242,#8243,#8244));
#2168=EDGE_LOOP('',(#8245,#8246,#8247,#8248));
#2169=EDGE_LOOP('',(#8249,#8250,#8251,#8252));
#2170=EDGE_LOOP('',(#8253));
#2171=EDGE_LOOP('',(#8254));
#2172=EDGE_LOOP('',(#8255,#8256,#8257,#8258));
#2173=EDGE_LOOP('',(#8259,#8260,#8261,#8262,#8263,#8264,#8265,#8266));
#2174=EDGE_LOOP('',(#8267));
#2175=EDGE_LOOP('',(#8268,#8269,#8270,#8271));
#2176=EDGE_LOOP('',(#8272,#8273,#8274,#8275));
#2177=EDGE_LOOP('',(#8276,#8277,#8278,#8279));
#2178=EDGE_LOOP('',(#8280,#8281,#8282,#8283));
#2179=EDGE_LOOP('',(#8284,#8285,#8286,#8287,#8288,#8289,#8290,#8291));
#2180=EDGE_LOOP('',(#8292));
#2181=EDGE_LOOP('',(#8293,#8294,#8295,#8296));
#2182=EDGE_LOOP('',(#8297,#8298,#8299,#8300));
#2183=EDGE_LOOP('',(#8301,#8302,#8303,#8304));
#2184=EDGE_LOOP('',(#8305,#8306,#8307,#8308));
#2185=EDGE_LOOP('',(#8309,#8310,#8311,#8312));
#2186=EDGE_LOOP('',(#8313));
#2187=EDGE_LOOP('',(#8314));
#2188=EDGE_LOOP('',(#8315,#8316,#8317,#8318));
#2189=EDGE_LOOP('',(#8319,#8320,#8321,#8322,#8323,#8324,#8325,#8326));
#2190=EDGE_LOOP('',(#8327));
#2191=EDGE_LOOP('',(#8328,#8329,#8330,#8331));
#2192=EDGE_LOOP('',(#8332));
#2193=EDGE_LOOP('',(#8333));
#2194=EDGE_LOOP('',(#8334,#8335,#8336,#8337));
#2195=EDGE_LOOP('',(#8338));
#2196=EDGE_LOOP('',(#8339));
#2197=EDGE_LOOP('',(#8340,#8341,#8342,#8343));
#2198=EDGE_LOOP('',(#8344,#8345,#8346,#8347));
#2199=EDGE_LOOP('',(#8348,#8349,#8350,#8351));
#2200=EDGE_LOOP('',(#8352,#8353,#8354,#8355));
#2201=EDGE_LOOP('',(#8356,#8357,#8358,#8359));
#2202=EDGE_LOOP('',(#8360));
#2203=EDGE_LOOP('',(#8361,#8362,#8363,#8364));
#2204=EDGE_LOOP('',(#8365,#8366,#8367,#8368));
#2205=EDGE_LOOP('',(#8369));
#2206=EDGE_LOOP('',(#8370,#8371,#8372,#8373));
#2207=EDGE_LOOP('',(#8374));
#2208=EDGE_LOOP('',(#8375));
#2209=EDGE_LOOP('',(#8376,#8377,#8378,#8379));
#2210=EDGE_LOOP('',(#8380));
#2211=EDGE_LOOP('',(#8381));
#2212=EDGE_LOOP('',(#8382,#8383,#8384,#8385));
#2213=EDGE_LOOP('',(#8386,#8387,#8388,#8389));
#2214=EDGE_LOOP('',(#8390));
#2215=EDGE_LOOP('',(#8391));
#2216=EDGE_LOOP('',(#8392));
#2217=EDGE_LOOP('',(#8393));
#2218=EDGE_LOOP('',(#8394,#8395,#8396,#8397));
#2219=EDGE_LOOP('',(#8398));
#2220=EDGE_LOOP('',(#8399));
#2221=EDGE_LOOP('',(#8400,#8401,#8402,#8403));
#2222=EDGE_LOOP('',(#8404));
#2223=EDGE_LOOP('',(#8405));
#2224=EDGE_LOOP('',(#8406,#8407,#8408,#8409));
#2225=EDGE_LOOP('',(#8410,#8411,#8412,#8413));
#2226=EDGE_LOOP('',(#8414,#8415,#8416,#8417));
#2227=EDGE_LOOP('',(#8418,#8419,#8420,#8421));
#2228=EDGE_LOOP('',(#8422,#8423,#8424,#8425));
#2229=EDGE_LOOP('',(#8426));
#2230=EDGE_LOOP('',(#8427,#8428,#8429,#8430));
#2231=EDGE_LOOP('',(#8431,#8432,#8433,#8434));
#2232=EDGE_LOOP('',(#8435));
#2233=EDGE_LOOP('',(#8436,#8437,#8438,#8439));
#2234=EDGE_LOOP('',(#8440));
#2235=EDGE_LOOP('',(#8441));
#2236=EDGE_LOOP('',(#8442,#8443,#8444,#8445));
#2237=EDGE_LOOP('',(#8446));
#2238=EDGE_LOOP('',(#8447));
#2239=EDGE_LOOP('',(#8448,#8449,#8450,#8451));
#2240=EDGE_LOOP('',(#8452,#8453,#8454,#8455));
#2241=EDGE_LOOP('',(#8456));
#2242=EDGE_LOOP('',(#8457));
#2243=EDGE_LOOP('',(#8458));
#2244=EDGE_LOOP('',(#8459));
#2245=EDGE_LOOP('',(#8460,#8461,#8462,#8463));
#2246=EDGE_LOOP('',(#8464,#8465,#8466,#8467));
#2247=EDGE_LOOP('',(#8468));
#2248=EDGE_LOOP('',(#8469));
#2249=EDGE_LOOP('',(#8470));
#2250=EDGE_LOOP('',(#8471));
#2251=EDGE_LOOP('',(#8472,#8473,#8474,#8475,#8476));
#2252=EDGE_LOOP('',(#8477,#8478,#8479,#8480,#8481));
#2253=EDGE_LOOP('',(#8482,#8483,#8484,#8485,#8486));
#2254=EDGE_LOOP('',(#8487,#8488));
#2255=EDGE_LOOP('',(#8489));
#2256=EDGE_LOOP('',(#8490,#8491,#8492,#8493,#8494));
#2257=EDGE_LOOP('',(#8495,#8496));
#2258=EDGE_LOOP('',(#8497));
#2259=EDGE_LOOP('',(#8498,#8499,#8500,#8501));
#2260=EDGE_LOOP('',(#8502,#8503,#8504,#8505));
#2261=EDGE_LOOP('',(#8506,#8507,#8508,#8509));
#2262=EDGE_LOOP('',(#8510,#8511,#8512,#8513));
#2263=EDGE_LOOP('',(#8514,#8515,#8516,#8517));
#2264=EDGE_LOOP('',(#8518,#8519,#8520,#8521,#8522,#8523,#8524,#8525,#8526,
#8527));
#2265=EDGE_LOOP('',(#8528,#8529,#8530,#8531,#8532,#8533));
#2266=EDGE_LOOP('',(#8534,#8535,#8536,#8537));
#2267=EDGE_LOOP('',(#8538,#8539,#8540,#8541,#8542,#8543,#8544));
#2268=EDGE_LOOP('',(#8545,#8546,#8547,#8548,#8549,#8550,#8551));
#2269=EDGE_LOOP('',(#8552,#8553,#8554,#8555,#8556,#8557));
#2270=EDGE_LOOP('',(#8558,#8559,#8560,#8561));
#2271=EDGE_LOOP('',(#8562));
#2272=EDGE_LOOP('',(#8563));
#2273=EDGE_LOOP('',(#8564,#8565,#8566,#8567));
#2274=EDGE_LOOP('',(#8568));
#2275=EDGE_LOOP('',(#8569));
#2276=EDGE_LOOP('',(#8570,#8571,#8572,#8573));
#2277=EDGE_LOOP('',(#8574));
#2278=EDGE_LOOP('',(#8575));
#2279=EDGE_LOOP('',(#8576,#8577,#8578,#8579));
#2280=EDGE_LOOP('',(#8580));
#2281=EDGE_LOOP('',(#8581));
#2282=EDGE_LOOP('',(#8582,#8583,#8584,#8585));
#2283=EDGE_LOOP('',(#8586));
#2284=EDGE_LOOP('',(#8587));
#2285=EDGE_LOOP('',(#8588,#8589,#8590,#8591));
#2286=EDGE_LOOP('',(#8592,#8593,#8594,#8595));
#2287=EDGE_LOOP('',(#8596,#8597,#8598,#8599));
#2288=EDGE_LOOP('',(#8600,#8601,#8602,#8603));
#2289=EDGE_LOOP('',(#8604,#8605,#8606,#8607));
#2290=EDGE_LOOP('',(#8608,#8609,#8610,#8611));
#2291=EDGE_LOOP('',(#8612,#8613,#8614,#8615));
#2292=EDGE_LOOP('',(#8616,#8617,#8618,#8619));
#2293=EDGE_LOOP('',(#8620,#8621,#8622,#8623));
#2294=EDGE_LOOP('',(#8624));
#2295=EDGE_LOOP('',(#8625));
#2296=EDGE_LOOP('',(#8626));
#2297=EDGE_LOOP('',(#8627));
#2298=EDGE_LOOP('',(#8628,#8629,#8630,#8631));
#2299=EDGE_LOOP('',(#8632,#8633,#8634,#8635));
#2300=EDGE_LOOP('',(#8636,#8637,#8638,#8639));
#2301=EDGE_LOOP('',(#8640,#8641,#8642,#8643));
#2302=EDGE_LOOP('',(#8644,#8645,#8646,#8647));
#2303=EDGE_LOOP('',(#8648,#8649,#8650,#8651));
#2304=EDGE_LOOP('',(#8652));
#2305=EDGE_LOOP('',(#8653));
#2306=EDGE_LOOP('',(#8654));
#2307=EDGE_LOOP('',(#8655));
#2308=EDGE_LOOP('',(#8656,#8657,#8658,#8659));
#2309=EDGE_LOOP('',(#8660,#8661,#8662,#8663,#8664,#8665,#8666,#8667,#8668,
#8669,#8670,#8671));
#2310=EDGE_LOOP('',(#8672,#8673,#8674,#8675,#8676,#8677,#8678,#8679,#8680,
#8681,#8682,#8683));
#2311=EDGE_LOOP('',(#8684,#8685,#8686,#8687,#8688,#8689));
#2312=EDGE_LOOP('',(#8690,#8691,#8692,#8693,#8694));
#2313=EDGE_LOOP('',(#8695,#8696,#8697,#8698));
#2314=EDGE_LOOP('',(#8699,#8700,#8701,#8702));
#2315=EDGE_LOOP('',(#8703));
#2316=EDGE_LOOP('',(#8704));
#2317=EDGE_LOOP('',(#8705,#8706,#8707,#8708,#8709));
#2318=EDGE_LOOP('',(#8710));
#2319=EDGE_LOOP('',(#8711));
#2320=EDGE_LOOP('',(#8712,#8713,#8714,#8715));
#2321=EDGE_LOOP('',(#8716,#8717,#8718,#8719,#8720,#8721));
#2322=EDGE_LOOP('',(#8722,#8723,#8724,#8725,#8726));
#2323=EDGE_LOOP('',(#8727));
#2324=EDGE_LOOP('',(#8728));
#2325=EDGE_LOOP('',(#8729,#8730,#8731,#8732));
#2326=EDGE_LOOP('',(#8733,#8734,#8735,#8736));
#2327=EDGE_LOOP('',(#8737,#8738,#8739,#8740));
#2328=EDGE_LOOP('',(#8741));
#2329=EDGE_LOOP('',(#8742));
#2330=EDGE_LOOP('',(#8743,#8744,#8745,#8746,#8747));
#2331=EDGE_LOOP('',(#8748,#8749));
#2332=EDGE_LOOP('',(#8750,#8751));
#2333=EDGE_LOOP('',(#8752,#8753));
#2334=EDGE_LOOP('',(#8754,#8755));
#2335=EDGE_LOOP('',(#8756,#8757));
#2336=EDGE_LOOP('',(#8758,#8759));
#2337=EDGE_LOOP('',(#8760,#8761));
#2338=EDGE_LOOP('',(#8762,#8763));
#2339=EDGE_LOOP('',(#8764,#8765,#8766,#8767));
#2340=EDGE_LOOP('',(#8768,#8769,#8770,#8771,#8772,#8773,#8774,#8775,#8776,
#8777,#8778,#8779,#8780,#8781,#8782,#8783,#8784,#8785,#8786,#8787));
#2341=EDGE_LOOP('',(#8788,#8789,#8790,#8791));
#2342=EDGE_LOOP('',(#8792,#8793,#8794,#8795));
#2343=EDGE_LOOP('',(#8796,#8797,#8798,#8799));
#2344=EDGE_LOOP('',(#8800,#8801,#8802,#8803));
#2345=EDGE_LOOP('',(#8804,#8805,#8806,#8807));
#2346=EDGE_LOOP('',(#8808,#8809,#8810,#8811,#8812,#8813));
#2347=EDGE_LOOP('',(#8814,#8815,#8816,#8817));
#2348=EDGE_LOOP('',(#8818,#8819,#8820,#8821));
#2349=EDGE_LOOP('',(#8822,#8823,#8824,#8825));
#2350=EDGE_LOOP('',(#8826,#8827,#8828,#8829));
#2351=EDGE_LOOP('',(#8830,#8831,#8832,#8833));
#2352=EDGE_LOOP('',(#8834,#8835,#8836,#8837));
#2353=EDGE_LOOP('',(#8838,#8839,#8840,#8841,#8842,#8843,#8844,#8845,#8846,
#8847,#8848,#8849,#8850,#8851,#8852,#8853,#8854,#8855,#8856,#8857));
#2354=EDGE_LOOP('',(#8858,#8859,#8860,#8861));
#2355=EDGE_LOOP('',(#8862,#8863,#8864,#8865));
#2356=EDGE_LOOP('',(#8866));
#2357=EDGE_LOOP('',(#8867));
#2358=EDGE_LOOP('',(#8868,#8869,#8870,#8871));
#2359=EDGE_LOOP('',(#8872));
#2360=EDGE_LOOP('',(#8873));
#2361=EDGE_LOOP('',(#8874,#8875,#8876,#8877));
#2362=EDGE_LOOP('',(#8878));
#2363=EDGE_LOOP('',(#8879));
#2364=EDGE_LOOP('',(#8880,#8881,#8882,#8883));
#2365=EDGE_LOOP('',(#8884));
#2366=EDGE_LOOP('',(#8885));
#2367=EDGE_LOOP('',(#8886,#8887,#8888,#8889));
#2368=EDGE_LOOP('',(#8890));
#2369=EDGE_LOOP('',(#8891));
#2370=EDGE_LOOP('',(#8892,#8893,#8894,#8895));
#2371=EDGE_LOOP('',(#8896,#8897,#8898,#8899));
#2372=EDGE_LOOP('',(#8900,#8901,#8902,#8903));
#2373=EDGE_LOOP('',(#8904,#8905,#8906,#8907));
#2374=EDGE_LOOP('',(#8908,#8909,#8910,#8911));
#2375=EDGE_LOOP('',(#8912,#8913,#8914,#8915));
#2376=EDGE_LOOP('',(#8916,#8917,#8918,#8919));
#2377=EDGE_LOOP('',(#8920,#8921,#8922,#8923));
#2378=EDGE_LOOP('',(#8924,#8925,#8926,#8927));
#2379=EDGE_LOOP('',(#8928,#8929,#8930,#8931));
#2380=EDGE_LOOP('',(#8932,#8933,#8934,#8935));
#2381=EDGE_LOOP('',(#8936,#8937,#8938,#8939));
#2382=EDGE_LOOP('',(#8940,#8941,#8942,#8943));
#2383=EDGE_LOOP('',(#8944,#8945,#8946,#8947));
#2384=EDGE_LOOP('',(#8948,#8949,#8950,#8951));
#2385=EDGE_LOOP('',(#8952,#8953,#8954,#8955));
#2386=EDGE_LOOP('',(#8956));
#2387=EDGE_LOOP('',(#8957));
#2388=EDGE_LOOP('',(#8958));
#2389=EDGE_LOOP('',(#8959));
#2390=EDGE_LOOP('',(#8960));
#2391=EDGE_LOOP('',(#8961));
#2392=EDGE_LOOP('',(#8962));
#2393=EDGE_LOOP('',(#8963));
#2394=EDGE_LOOP('',(#8964));
#2395=EDGE_LOOP('',(#8965));
#2396=EDGE_LOOP('',(#8966,#8967,#8968,#8969));
#2397=EDGE_LOOP('',(#8970));
#2398=EDGE_LOOP('',(#8971));
#2399=EDGE_LOOP('',(#8972));
#2400=EDGE_LOOP('',(#8973));
#2401=EDGE_LOOP('',(#8974));
#2402=EDGE_LOOP('',(#8975));
#2403=EDGE_LOOP('',(#8976));
#2404=EDGE_LOOP('',(#8977));
#2405=EDGE_LOOP('',(#8978));
#2406=EDGE_LOOP('',(#8979));
#2407=EDGE_LOOP('',(#8980,#8981,#8982,#8983));
#2408=EDGE_LOOP('',(#8984,#8985,#8986,#8987));
#2409=EDGE_LOOP('',(#8988,#8989,#8990,#8991));
#2410=EDGE_LOOP('',(#8992,#8993,#8994,#8995));
#2411=EDGE_LOOP('',(#8996,#8997,#8998,#8999));
#2412=EDGE_LOOP('',(#9000,#9001));
#2413=EDGE_LOOP('',(#9002,#9003,#9004,#9005));
#2414=EDGE_LOOP('',(#9006,#9007));
#2415=EDGE_LOOP('',(#9008,#9009,#9010,#9011));
#2416=EDGE_LOOP('',(#9012,#9013));
#2417=EDGE_LOOP('',(#9014,#9015,#9016,#9017));
#2418=EDGE_LOOP('',(#9018,#9019));
#2419=EDGE_LOOP('',(#9020,#9021,#9022,#9023));
#2420=EDGE_LOOP('',(#9024,#9025,#9026,#9027,#9028,#9029,#9030,#9031,#9032,
#9033,#9034,#9035,#9036,#9037,#9038,#9039));
#2421=EDGE_LOOP('',(#9040));
#2422=EDGE_LOOP('',(#9041));
#2423=EDGE_LOOP('',(#9042));
#2424=EDGE_LOOP('',(#9043));
#2425=EDGE_LOOP('',(#9044));
#2426=EDGE_LOOP('',(#9045,#9046,#9047,#9048,#9049,#9050,#9051,#9052,#9053,
#9054,#9055,#9056,#9057,#9058,#9059,#9060));
#2427=EDGE_LOOP('',(#9061));
#2428=EDGE_LOOP('',(#9062));
#2429=EDGE_LOOP('',(#9063));
#2430=EDGE_LOOP('',(#9064));
#2431=EDGE_LOOP('',(#9065));
#2432=EDGE_LOOP('',(#9066,#9067,#9068,#9069));
#2433=EDGE_LOOP('',(#9070,#9071,#9072,#9073));
#2434=EDGE_LOOP('',(#9074,#9075,#9076,#9077));
#2435=EDGE_LOOP('',(#9078,#9079,#9080,#9081));
#2436=EDGE_LOOP('',(#9082,#9083,#9084,#9085));
#2437=EDGE_LOOP('',(#9086));
#2438=EDGE_LOOP('',(#9087));
#2439=EDGE_LOOP('',(#9088,#9089,#9090,#9091));
#2440=EDGE_LOOP('',(#9092));
#2441=EDGE_LOOP('',(#9093));
#2442=EDGE_LOOP('',(#9094,#9095,#9096,#9097));
#2443=EDGE_LOOP('',(#9098,#9099,#9100,#9101));
#2444=EDGE_LOOP('',(#9102,#9103,#9104,#9105));
#2445=EDGE_LOOP('',(#9106,#9107,#9108,#9109));
#2446=EDGE_LOOP('',(#9110,#9111,#9112,#9113));
#2447=EDGE_LOOP('',(#9114,#9115,#9116,#9117,#9118,#9119,#9120,#9121,#9122,
#9123,#9124,#9125));
#2448=EDGE_LOOP('',(#9126));
#2449=EDGE_LOOP('',(#9127));
#2450=EDGE_LOOP('',(#9128));
#2451=EDGE_LOOP('',(#9129));
#2452=EDGE_LOOP('',(#9130,#9131,#9132,#9133));
#2453=EDGE_LOOP('',(#9134,#9135,#9136,#9137));
#2454=EDGE_LOOP('',(#9138));
#2455=EDGE_LOOP('',(#9139));
#2456=EDGE_LOOP('',(#9140));
#2457=EDGE_LOOP('',(#9141));
#2458=EDGE_LOOP('',(#9142,#9143,#9144,#9145));
#2459=EDGE_LOOP('',(#9146,#9147,#9148,#9149));
#2460=EDGE_LOOP('',(#9150,#9151,#9152,#9153));
#2461=EDGE_LOOP('',(#9154,#9155,#9156,#9157));
#2462=EDGE_LOOP('',(#9158,#9159,#9160,#9161,#9162,#9163,#9164,#9165));
#2463=EDGE_LOOP('',(#9166));
#2464=EDGE_LOOP('',(#9167,#9168,#9169,#9170));
#2465=EDGE_LOOP('',(#9171,#9172,#9173,#9174));
#2466=EDGE_LOOP('',(#9175,#9176,#9177,#9178));
#2467=EDGE_LOOP('',(#9179,#9180,#9181,#9182));
#2468=EDGE_LOOP('',(#9183,#9184,#9185,#9186));
#2469=EDGE_LOOP('',(#9187));
#2470=EDGE_LOOP('',(#9188));
#2471=EDGE_LOOP('',(#9189,#9190,#9191,#9192));
#2472=EDGE_LOOP('',(#9193,#9194,#9195,#9196,#9197,#9198,#9199,#9200));
#2473=EDGE_LOOP('',(#9201));
#2474=EDGE_LOOP('',(#9202,#9203,#9204,#9205));
#2475=EDGE_LOOP('',(#9206,#9207,#9208,#9209));
#2476=EDGE_LOOP('',(#9210,#9211,#9212,#9213));
#2477=EDGE_LOOP('',(#9214,#9215,#9216,#9217));
#2478=EDGE_LOOP('',(#9218,#9219,#9220,#9221,#9222,#9223,#9224,#9225));
#2479=EDGE_LOOP('',(#9226));
#2480=EDGE_LOOP('',(#9227,#9228,#9229,#9230));
#2481=EDGE_LOOP('',(#9231,#9232,#9233,#9234));
#2482=EDGE_LOOP('',(#9235,#9236,#9237,#9238));
#2483=EDGE_LOOP('',(#9239,#9240,#9241,#9242));
#2484=EDGE_LOOP('',(#9243,#9244,#9245,#9246));
#2485=EDGE_LOOP('',(#9247));
#2486=EDGE_LOOP('',(#9248));
#2487=EDGE_LOOP('',(#9249,#9250,#9251,#9252));
#2488=EDGE_LOOP('',(#9253,#9254,#9255,#9256,#9257,#9258,#9259,#9260));
#2489=EDGE_LOOP('',(#9261));
#2490=EDGE_LOOP('',(#9262,#9263,#9264,#9265));
#2491=EDGE_LOOP('',(#9266));
#2492=EDGE_LOOP('',(#9267,#9268,#9269,#9270));
#2493=EDGE_LOOP('',(#9271));
#2494=EDGE_LOOP('',(#9272,#9273,#9274,#9275));
#2495=EDGE_LOOP('',(#9276,#9277,#9278,#9279));
#2496=EDGE_LOOP('',(#9280,#9281,#9282,#9283));
#2497=EDGE_LOOP('',(#9284));
#2498=EDGE_LOOP('',(#9285,#9286,#9287,#9288));
#2499=EDGE_LOOP('',(#9289,#9290,#9291,#9292));
#2500=EDGE_LOOP('',(#9293));
#2501=EDGE_LOOP('',(#9294,#9295,#9296,#9297));
#2502=EDGE_LOOP('',(#9298,#9299,#9300,#9301));
#2503=EDGE_LOOP('',(#9302));
#2504=EDGE_LOOP('',(#9303));
#2505=EDGE_LOOP('',(#9304));
#2506=EDGE_LOOP('',(#9305,#9306,#9307,#9308));
#2507=EDGE_LOOP('',(#9309));
#2508=EDGE_LOOP('',(#9310,#9311));
#2509=EDGE_LOOP('',(#9312,#9313,#9314,#9315,#9316,#9317,#9318,#9319,#9320));
#2510=EDGE_LOOP('',(#9321,#9322));
#2511=EDGE_LOOP('',(#9323,#9324,#9325,#9326,#9327,#9328,#9329,#9330,#9331,
#9332,#9333,#9334));
#2512=EDGE_LOOP('',(#9335,#9336,#9337,#9338));
#2513=EDGE_LOOP('',(#9339,#9340,#9341,#9342));
#2514=EDGE_LOOP('',(#9343));
#2515=EDGE_LOOP('',(#9344,#9345,#9346,#9347));
#2516=EDGE_LOOP('',(#9348,#9349,#9350,#9351));
#2517=EDGE_LOOP('',(#9352));
#2518=EDGE_LOOP('',(#9353,#9354,#9355,#9356));
#2519=EDGE_LOOP('',(#9357));
#2520=EDGE_LOOP('',(#9358,#9359,#9360,#9361));
#2521=EDGE_LOOP('',(#9362,#9363));
#2522=EDGE_LOOP('',(#9364,#9365,#9366,#9367,#9368,#9369,#9370,#9371));
#2523=EDGE_LOOP('',(#9372,#9373));
#2524=EDGE_LOOP('',(#9374,#9375,#9376,#9377,#9378,#9379,#9380,#9381));
#2525=EDGE_LOOP('',(#9382,#9383));
#2526=EDGE_LOOP('',(#9384,#9385,#9386,#9387,#9388,#9389,#9390,#9391));
#2527=EDGE_LOOP('',(#9392,#9393));
#2528=EDGE_LOOP('',(#9394,#9395,#9396,#9397,#9398,#9399,#9400,#9401));
#2529=EDGE_LOOP('',(#9402,#9403,#9404,#9405,#9406,#9407,#9408,#9409,#9410,
#9411,#9412,#9413));
#2530=EDGE_LOOP('',(#9414,#9415,#9416,#9417,#9418,#9419,#9420,#9421,#9422,
#9423,#9424,#9425));
#2531=EDGE_LOOP('',(#9426,#9427,#9428,#9429,#9430,#9431,#9432,#9433,#9434,
#9435,#9436,#9437));
#2532=EDGE_LOOP('',(#9438,#9439,#9440,#9441,#9442,#9443,#9444,#9445,#9446,
#9447));
#2533=EDGE_LOOP('',(#9448,#9449,#9450,#9451));
#2534=EDGE_LOOP('',(#9452,#9453,#9454,#9455));
#2535=EDGE_LOOP('',(#9456));
#2536=EDGE_LOOP('',(#9457));
#2537=EDGE_LOOP('',(#9458));
#2538=EDGE_LOOP('',(#9459));
#2539=EDGE_LOOP('',(#9460,#9461,#9462,#9463));
#2540=EDGE_LOOP('',(#9464,#9465,#9466,#9467,#9468,#9469,#9470,#9471,#9472,
#9473));
#2541=EDGE_LOOP('',(#9474,#9475,#9476,#9477));
#2542=EDGE_LOOP('',(#9478,#9479,#9480,#9481));
#2543=EDGE_LOOP('',(#9482,#9483,#9484,#9485));
#2544=EDGE_LOOP('',(#9486,#9487,#9488,#9489));
#2545=EDGE_LOOP('',(#9490,#9491,#9492,#9493));
#2546=EDGE_LOOP('',(#9494,#9495,#9496,#9497,#9498,#9499,#9500,#9501,#9502,
#9503,#9504,#9505));
#2547=EDGE_LOOP('',(#9506,#9507,#9508,#9509));
#2548=EDGE_LOOP('',(#9510,#9511,#9512,#9513));
#2549=EDGE_LOOP('',(#9514,#9515,#9516,#9517));
#2550=EDGE_LOOP('',(#9518,#9519,#9520,#9521));
#2551=EDGE_LOOP('',(#9522,#9523,#9524,#9525));
#2552=EDGE_LOOP('',(#9526,#9527,#9528,#9529));
#2553=EDGE_LOOP('',(#9530,#9531,#9532,#9533));
#2554=EDGE_LOOP('',(#9534,#9535,#9536,#9537));
#2555=EDGE_LOOP('',(#9538,#9539,#9540,#9541,#9542,#9543,#9544,#9545));
#2556=EDGE_LOOP('',(#9546,#9547,#9548,#9549,#9550,#9551,#9552,#9553));
#2557=EDGE_LOOP('',(#9554,#9555,#9556,#9557));
#2558=EDGE_LOOP('',(#9558,#9559,#9560,#9561));
#2559=EDGE_LOOP('',(#9562,#9563,#9564,#9565));
#2560=EDGE_LOOP('',(#9566,#9567,#9568,#9569));
#2561=EDGE_LOOP('',(#9570,#9571,#9572,#9573));
#2562=EDGE_LOOP('',(#9574,#9575,#9576,#9577));
#2563=EDGE_LOOP('',(#9578,#9579,#9580,#9581));
#2564=EDGE_LOOP('',(#9582,#9583,#9584,#9585));
#2565=EDGE_LOOP('',(#9586,#9587,#9588,#9589,#9590,#9591,#9592,#9593));
#2566=EDGE_LOOP('',(#9594,#9595,#9596,#9597,#9598,#9599,#9600,#9601));
#2567=EDGE_LOOP('',(#9602,#9603,#9604,#9605));
#2568=EDGE_LOOP('',(#9606,#9607,#9608,#9609));
#2569=EDGE_LOOP('',(#9610,#9611,#9612,#9613));
#2570=EDGE_LOOP('',(#9614,#9615,#9616,#9617));
#2571=EDGE_LOOP('',(#9618,#9619,#9620,#9621));
#2572=EDGE_LOOP('',(#9622,#9623,#9624,#9625));
#2573=EDGE_LOOP('',(#9626,#9627,#9628,#9629,#9630,#9631));
#2574=EDGE_LOOP('',(#9632,#9633,#9634,#9635,#9636,#9637));
#2575=EDGE_LOOP('',(#9638));
#2576=EDGE_LOOP('',(#9639));
#2577=EDGE_LOOP('',(#9640,#9641,#9642,#9643));
#2578=EDGE_LOOP('',(#9644,#9645,#9646,#9647));
#2579=EDGE_LOOP('',(#9648,#9649,#9650,#9651));
#2580=EDGE_LOOP('',(#9652));
#2581=EDGE_LOOP('',(#9653));
#2582=EDGE_LOOP('',(#9654,#9655,#9656,#9657));
#2583=EDGE_LOOP('',(#9658,#9659,#9660,#9661));
#2584=EDGE_LOOP('',(#9662,#9663,#9664,#9665,#9666,#9667));
#2585=EDGE_LOOP('',(#9668,#9669,#9670,#9671,#9672));
#2586=EDGE_LOOP('',(#9673,#9674,#9675,#9676));
#2587=EDGE_LOOP('',(#9677,#9678,#9679,#9680));
#2588=EDGE_LOOP('',(#9681));
#2589=EDGE_LOOP('',(#9682));
#2590=EDGE_LOOP('',(#9683,#9684,#9685,#9686,#9687));
#2591=EDGE_LOOP('',(#9688));
#2592=EDGE_LOOP('',(#9689));
#2593=EDGE_LOOP('',(#9690,#9691,#9692,#9693));
#2594=EDGE_LOOP('',(#9694,#9695,#9696,#9697,#9698,#9699));
#2595=EDGE_LOOP('',(#9700,#9701,#9702,#9703,#9704));
#2596=EDGE_LOOP('',(#9705));
#2597=EDGE_LOOP('',(#9706));
#2598=EDGE_LOOP('',(#9707,#9708,#9709,#9710));
#2599=EDGE_LOOP('',(#9711,#9712,#9713,#9714));
#2600=EDGE_LOOP('',(#9715,#9716,#9717,#9718));
#2601=EDGE_LOOP('',(#9719));
#2602=EDGE_LOOP('',(#9720));
#2603=EDGE_LOOP('',(#9721,#9722,#9723,#9724,#9725));
#2604=EDGE_LOOP('',(#9726,#9727));
#2605=EDGE_LOOP('',(#9728,#9729));
#2606=EDGE_LOOP('',(#9730,#9731));
#2607=EDGE_LOOP('',(#9732,#9733));
#2608=EDGE_LOOP('',(#9734,#9735));
#2609=EDGE_LOOP('',(#9736,#9737));
#2610=EDGE_LOOP('',(#9738,#9739));
#2611=EDGE_LOOP('',(#9740,#9741,#9742,#9743));
#2612=EDGE_LOOP('',(#9744,#9745,#9746,#9747,#9748,#9749,#9750,#9751,#9752,
#9753,#9754,#9755,#9756,#9757,#9758,#9759,#9760,#9761));
#2613=EDGE_LOOP('',(#9762,#9763,#9764,#9765));
#2614=EDGE_LOOP('',(#9766,#9767,#9768,#9769));
#2615=EDGE_LOOP('',(#9770,#9771,#9772,#9773));
#2616=EDGE_LOOP('',(#9774,#9775,#9776,#9777));
#2617=EDGE_LOOP('',(#9778,#9779,#9780,#9781,#9782,#9783));
#2618=EDGE_LOOP('',(#9784,#9785,#9786,#9787));
#2619=EDGE_LOOP('',(#9788,#9789,#9790,#9791));
#2620=EDGE_LOOP('',(#9792,#9793,#9794,#9795));
#2621=EDGE_LOOP('',(#9796,#9797,#9798,#9799));
#2622=EDGE_LOOP('',(#9800,#9801,#9802,#9803));
#2623=EDGE_LOOP('',(#9804,#9805,#9806,#9807,#9808,#9809,#9810,#9811,#9812,
#9813,#9814,#9815,#9816,#9817,#9818,#9819,#9820,#9821));
#2624=EDGE_LOOP('',(#9822,#9823,#9824,#9825));
#2625=EDGE_LOOP('',(#9826,#9827,#9828,#9829));
#2626=EDGE_LOOP('',(#9830));
#2627=EDGE_LOOP('',(#9831));
#2628=EDGE_LOOP('',(#9832,#9833,#9834,#9835));
#2629=EDGE_LOOP('',(#9836));
#2630=EDGE_LOOP('',(#9837));
#2631=EDGE_LOOP('',(#9838,#9839,#9840,#9841));
#2632=EDGE_LOOP('',(#9842));
#2633=EDGE_LOOP('',(#9843));
#2634=EDGE_LOOP('',(#9844,#9845,#9846,#9847));
#2635=EDGE_LOOP('',(#9848));
#2636=EDGE_LOOP('',(#9849));
#2637=EDGE_LOOP('',(#9850,#9851,#9852,#9853));
#2638=EDGE_LOOP('',(#9854));
#2639=EDGE_LOOP('',(#9855));
#2640=EDGE_LOOP('',(#9856,#9857,#9858,#9859));
#2641=EDGE_LOOP('',(#9860,#9861,#9862,#9863));
#2642=EDGE_LOOP('',(#9864,#9865,#9866,#9867));
#2643=EDGE_LOOP('',(#9868,#9869,#9870,#9871));
#2644=EDGE_LOOP('',(#9872,#9873,#9874,#9875));
#2645=EDGE_LOOP('',(#9876,#9877,#9878,#9879));
#2646=EDGE_LOOP('',(#9880,#9881,#9882,#9883));
#2647=EDGE_LOOP('',(#9884,#9885,#9886,#9887,#9888,#9889));
#2648=EDGE_LOOP('',(#9890,#9891,#9892,#9893,#9894,#9895));
#2649=EDGE_LOOP('',(#9896));
#2650=EDGE_LOOP('',(#9897));
#2651=EDGE_LOOP('',(#9898,#9899,#9900,#9901));
#2652=EDGE_LOOP('',(#9902,#9903,#9904,#9905));
#2653=EDGE_LOOP('',(#9906,#9907,#9908,#9909));
#2654=EDGE_LOOP('',(#9910));
#2655=EDGE_LOOP('',(#9911));
#2656=EDGE_LOOP('',(#9912,#9913,#9914,#9915));
#2657=EDGE_LOOP('',(#9916,#9917,#9918,#9919));
#2658=EDGE_LOOP('',(#9920,#9921,#9922,#9923));
#2659=EDGE_LOOP('',(#9924));
#2660=EDGE_LOOP('',(#9925));
#2661=EDGE_LOOP('',(#9926));
#2662=EDGE_LOOP('',(#9927));
#2663=EDGE_LOOP('',(#9928));
#2664=EDGE_LOOP('',(#9929,#9930,#9931,#9932));
#2665=EDGE_LOOP('',(#9933,#9934,#9935,#9936));
#2666=EDGE_LOOP('',(#9937,#9938,#9939,#9940));
#2667=EDGE_LOOP('',(#9941));
#2668=EDGE_LOOP('',(#9942));
#2669=EDGE_LOOP('',(#9943,#9944,#9945,#9946));
#2670=EDGE_LOOP('',(#9947));
#2671=EDGE_LOOP('',(#9948));
#2672=EDGE_LOOP('',(#9949));
#2673=EDGE_LOOP('',(#9950,#9951,#9952,#9953));
#2674=EDGE_LOOP('',(#9954));
#2675=EDGE_LOOP('',(#9955));
#2676=EDGE_LOOP('',(#9956,#9957,#9958,#9959));
#2677=EDGE_LOOP('',(#9960,#9961,#9962,#9963));
#2678=EDGE_LOOP('',(#9964));
#2679=EDGE_LOOP('',(#9965));
#2680=EDGE_LOOP('',(#9966));
#2681=EDGE_LOOP('',(#9967));
#2682=EDGE_LOOP('',(#9968,#9969,#9970,#9971));
#2683=EDGE_LOOP('',(#9972,#9973,#9974,#9975));
#2684=EDGE_LOOP('',(#9976));
#2685=EDGE_LOOP('',(#9977));
#2686=EDGE_LOOP('',(#9978));
#2687=EDGE_LOOP('',(#9979));
#2688=EDGE_LOOP('',(#9980,#9981,#9982,#9983));
#2689=EDGE_LOOP('',(#9984));
#2690=EDGE_LOOP('',(#9985));
#2691=EDGE_LOOP('',(#9986,#9987,#9988,#9989));
#2692=EDGE_LOOP('',(#9990));
#2693=EDGE_LOOP('',(#9991));
#2694=EDGE_LOOP('',(#9992,#9993,#9994,#9995));
#2695=EDGE_LOOP('',(#9996,#9997,#9998,#9999));
#2696=EDGE_LOOP('',(#10000));
#2697=EDGE_LOOP('',(#10001));
#2698=EDGE_LOOP('',(#10002));
#2699=EDGE_LOOP('',(#10003));
#2700=EDGE_LOOP('',(#10004,#10005,#10006,#10007,#10008,#10009,#10010,#10011,
#10012));
#2701=EDGE_LOOP('',(#10013,#10014,#10015,#10016,#10017,#10018,#10019));
#2702=EDGE_LOOP('',(#10020,#10021,#10022,#10023,#10024,#10025,#10026,#10027,
#10028));
#2703=EDGE_LOOP('',(#10029,#10030,#10031));
#2704=EDGE_LOOP('',(#10032,#10033,#10034));
#2705=EDGE_LOOP('',(#10035,#10036,#10037));
#2706=EDGE_LOOP('',(#10038,#10039,#10040,#10041,#10042,#10043,#10044));
#2707=EDGE_LOOP('',(#10045,#10046,#10047,#10048,#10049,#10050,#10051));
#2708=EDGE_LOOP('',(#10052,#10053,#10054,#10055,#10056,#10057,#10058,#10059,
#10060,#10061));
#2709=EDGE_LOOP('',(#10062,#10063));
#2710=EDGE_LOOP('',(#10064,#10065));
#2711=EDGE_LOOP('',(#10066,#10067));
#2712=EDGE_LOOP('',(#10068));
#2713=EDGE_LOOP('',(#10069));
#2714=EDGE_LOOP('',(#10070));
#2715=EDGE_LOOP('',(#10071,#10072,#10073,#10074,#10075,#10076,#10077,#10078,
#10079,#10080,#10081,#10082,#10083,#10084,#10085,#10086,#10087,#10088,#10089,
#10090,#10091,#10092,#10093,#10094,#10095,#10096,#10097,#10098,#10099,#10100,
#10101,#10102,#10103,#10104,#10105,#10106,#10107,#10108,#10109,#10110));
#2716=EDGE_LOOP('',(#10111,#10112,#10113,#10114));
#2717=EDGE_LOOP('',(#10115));
#2718=EDGE_LOOP('',(#10116));
#2719=EDGE_LOOP('',(#10117));
#2720=EDGE_LOOP('',(#10118,#10119,#10120,#10121,#10122,#10123,#10124,#10125,
#10126,#10127,#10128,#10129,#10130,#10131,#10132,#10133,#10134,#10135,#10136,
#10137,#10138,#10139,#10140,#10141,#10142,#10143,#10144,#10145,#10146,#10147,
#10148,#10149,#10150,#10151,#10152,#10153,#10154,#10155,#10156,#10157));
#2721=EDGE_LOOP('',(#10158,#10159,#10160,#10161));
#2722=EDGE_LOOP('',(#10162));
#2723=EDGE_LOOP('',(#10163));
#2724=EDGE_LOOP('',(#10164,#10165,#10166,#10167));
#2725=EDGE_LOOP('',(#10168,#10169,#10170,#10171));
#2726=EDGE_LOOP('',(#10172,#10173,#10174,#10175));
#2727=EDGE_LOOP('',(#10176,#10177,#10178,#10179));
#2728=EDGE_LOOP('',(#10180,#10181,#10182,#10183));
#2729=EDGE_LOOP('',(#10184,#10185,#10186,#10187));
#2730=EDGE_LOOP('',(#10188,#10189,#10190,#10191));
#2731=EDGE_LOOP('',(#10192,#10193,#10194,#10195));
#2732=EDGE_LOOP('',(#10196,#10197,#10198,#10199));
#2733=EDGE_LOOP('',(#10200,#10201,#10202,#10203));
#2734=EDGE_LOOP('',(#10204,#10205,#10206,#10207));
#2735=EDGE_LOOP('',(#10208,#10209,#10210,#10211));
#2736=EDGE_LOOP('',(#10212,#10213,#10214,#10215));
#2737=EDGE_LOOP('',(#10216,#10217,#10218,#10219));
#2738=EDGE_LOOP('',(#10220,#10221,#10222,#10223));
#2739=EDGE_LOOP('',(#10224,#10225,#10226,#10227));
#2740=EDGE_LOOP('',(#10228,#10229,#10230,#10231));
#2741=EDGE_LOOP('',(#10232,#10233,#10234,#10235));
#2742=EDGE_LOOP('',(#10236,#10237,#10238,#10239));
#2743=EDGE_LOOP('',(#10240,#10241,#10242,#10243));
#2744=EDGE_LOOP('',(#10244,#10245,#10246,#10247));
#2745=EDGE_LOOP('',(#10248,#10249,#10250,#10251));
#2746=EDGE_LOOP('',(#10252,#10253,#10254,#10255));
#2747=EDGE_LOOP('',(#10256,#10257,#10258,#10259));
#2748=EDGE_LOOP('',(#10260,#10261,#10262,#10263));
#2749=EDGE_LOOP('',(#10264,#10265,#10266,#10267));
#2750=EDGE_LOOP('',(#10268,#10269,#10270,#10271));
#2751=EDGE_LOOP('',(#10272,#10273,#10274,#10275));
#2752=EDGE_LOOP('',(#10276,#10277,#10278,#10279));
#2753=EDGE_LOOP('',(#10280,#10281,#10282,#10283));
#2754=EDGE_LOOP('',(#10284,#10285,#10286,#10287));
#2755=EDGE_LOOP('',(#10288,#10289,#10290,#10291));
#2756=EDGE_LOOP('',(#10292,#10293,#10294,#10295));
#2757=EDGE_LOOP('',(#10296,#10297,#10298,#10299));
#2758=EDGE_LOOP('',(#10300,#10301,#10302,#10303));
#2759=EDGE_LOOP('',(#10304,#10305,#10306,#10307));
#2760=EDGE_LOOP('',(#10308,#10309,#10310,#10311));
#2761=EDGE_LOOP('',(#10312,#10313,#10314,#10315));
#2762=EDGE_LOOP('',(#10316,#10317,#10318,#10319));
#2763=EDGE_LOOP('',(#10320,#10321,#10322,#10323));
#2764=EDGE_LOOP('',(#10324,#10325,#10326,#10327));
#2765=EDGE_LOOP('',(#10328));
#2766=EDGE_LOOP('',(#10329));
#2767=EDGE_LOOP('',(#10330));
#2768=EDGE_LOOP('',(#10331));
#2769=EDGE_LOOP('',(#10332));
#2770=EDGE_LOOP('',(#10333,#10334,#10335,#10336));
#2771=EDGE_LOOP('',(#10337,#10338,#10339,#10340));
#2772=EDGE_LOOP('',(#10341));
#2773=EDGE_LOOP('',(#10342));
#2774=EDGE_LOOP('',(#10343,#10344,#10345,#10346));
#2775=EDGE_LOOP('',(#10347));
#2776=EDGE_LOOP('',(#10348,#10349,#10350,#10351));
#2777=EDGE_LOOP('',(#10352,#10353,#10354,#10355));
#2778=EDGE_LOOP('',(#10356));
#2779=EDGE_LOOP('',(#10357));
#2780=EDGE_LOOP('',(#10358));
#2781=EDGE_LOOP('',(#10359));
#2782=EDGE_LOOP('',(#10360,#10361,#10362,#10363));
#2783=EDGE_LOOP('',(#10364,#10365,#10366,#10367));
#2784=EDGE_LOOP('',(#10368));
#2785=EDGE_LOOP('',(#10369));
#2786=EDGE_LOOP('',(#10370));
#2787=EDGE_LOOP('',(#10371));
#2788=EDGE_LOOP('',(#10372,#10373,#10374,#10375));
#2789=EDGE_LOOP('',(#10376));
#2790=EDGE_LOOP('',(#10377));
#2791=EDGE_LOOP('',(#10378,#10379,#10380,#10381));
#2792=EDGE_LOOP('',(#10382));
#2793=EDGE_LOOP('',(#10383));
#2794=EDGE_LOOP('',(#10384,#10385,#10386,#10387));
#2795=EDGE_LOOP('',(#10388,#10389,#10390,#10391));
#2796=EDGE_LOOP('',(#10392));
#2797=EDGE_LOOP('',(#10393));
#2798=EDGE_LOOP('',(#10394));
#2799=EDGE_LOOP('',(#10395));
#2800=EDGE_LOOP('',(#10396,#10397,#10398,#10399,#10400,#10401,#10402,#10403,
#10404));
#2801=EDGE_LOOP('',(#10405,#10406,#10407,#10408,#10409,#10410,#10411));
#2802=EDGE_LOOP('',(#10412,#10413,#10414,#10415,#10416,#10417,#10418,#10419,
#10420));
#2803=EDGE_LOOP('',(#10421,#10422,#10423));
#2804=EDGE_LOOP('',(#10424,#10425,#10426));
#2805=EDGE_LOOP('',(#10427,#10428,#10429));
#2806=EDGE_LOOP('',(#10430,#10431,#10432,#10433,#10434,#10435,#10436));
#2807=EDGE_LOOP('',(#10437,#10438,#10439,#10440,#10441,#10442,#10443));
#2808=EDGE_LOOP('',(#10444,#10445,#10446,#10447,#10448,#10449,#10450,#10451,
#10452,#10453));
#2809=EDGE_LOOP('',(#10454,#10455));
#2810=EDGE_LOOP('',(#10456,#10457));
#2811=EDGE_LOOP('',(#10458,#10459));
#2812=EDGE_LOOP('',(#10460));
#2813=EDGE_LOOP('',(#10461));
#2814=EDGE_LOOP('',(#10462));
#2815=EDGE_LOOP('',(#10463,#10464,#10465,#10466,#10467,#10468,#10469,#10470,
#10471,#10472,#10473,#10474,#10475,#10476,#10477,#10478,#10479,#10480,#10481,
#10482,#10483,#10484,#10485,#10486,#10487,#10488,#10489,#10490,#10491,#10492,
#10493,#10494,#10495,#10496,#10497,#10498,#10499,#10500,#10501,#10502,#10503,
#10504,#10505,#10506,#10507,#10508,#10509,#10510,#10511,#10512,#10513,#10514,
#10515,#10516,#10517,#10518,#10519,#10520,#10521,#10522,#10523,#10524,#10525,
#10526,#10527,#10528,#10529,#10530,#10531,#10532,#10533,#10534,#10535,#10536,
#10537,#10538,#10539,#10540,#10541,#10542));
#2816=EDGE_LOOP('',(#10543,#10544,#10545,#10546));
#2817=EDGE_LOOP('',(#10547));
#2818=EDGE_LOOP('',(#10548));
#2819=EDGE_LOOP('',(#10549));
#2820=EDGE_LOOP('',(#10550,#10551,#10552,#10553,#10554,#10555,#10556,#10557,
#10558,#10559,#10560,#10561,#10562,#10563,#10564,#10565,#10566,#10567,#10568,
#10569,#10570,#10571,#10572,#10573,#10574,#10575,#10576,#10577,#10578,#10579,
#10580,#10581,#10582,#10583,#10584,#10585,#10586,#10587,#10588,#10589,#10590,
#10591,#10592,#10593,#10594,#10595,#10596,#10597,#10598,#10599,#10600,#10601,
#10602,#10603,#10604,#10605,#10606,#10607,#10608,#10609,#10610,#10611,#10612,
#10613,#10614,#10615,#10616,#10617,#10618,#10619,#10620,#10621,#10622,#10623,
#10624,#10625,#10626,#10627,#10628,#10629));
#2821=EDGE_LOOP('',(#10630,#10631,#10632,#10633));
#2822=EDGE_LOOP('',(#10634));
#2823=EDGE_LOOP('',(#10635));
#2824=EDGE_LOOP('',(#10636,#10637,#10638,#10639));
#2825=EDGE_LOOP('',(#10640,#10641,#10642,#10643));
#2826=EDGE_LOOP('',(#10644,#10645,#10646,#10647));
#2827=EDGE_LOOP('',(#10648,#10649,#10650,#10651));
#2828=EDGE_LOOP('',(#10652,#10653,#10654,#10655));
#2829=EDGE_LOOP('',(#10656,#10657,#10658,#10659));
#2830=EDGE_LOOP('',(#10660,#10661,#10662,#10663));
#2831=EDGE_LOOP('',(#10664,#10665,#10666,#10667));
#2832=EDGE_LOOP('',(#10668,#10669,#10670,#10671));
#2833=EDGE_LOOP('',(#10672,#10673,#10674,#10675));
#2834=EDGE_LOOP('',(#10676,#10677,#10678,#10679));
#2835=EDGE_LOOP('',(#10680,#10681,#10682,#10683));
#2836=EDGE_LOOP('',(#10684,#10685,#10686,#10687));
#2837=EDGE_LOOP('',(#10688,#10689,#10690,#10691));
#2838=EDGE_LOOP('',(#10692,#10693,#10694,#10695));
#2839=EDGE_LOOP('',(#10696,#10697,#10698,#10699));
#2840=EDGE_LOOP('',(#10700,#10701,#10702,#10703));
#2841=EDGE_LOOP('',(#10704,#10705,#10706,#10707));
#2842=EDGE_LOOP('',(#10708,#10709,#10710,#10711));
#2843=EDGE_LOOP('',(#10712,#10713,#10714,#10715));
#2844=EDGE_LOOP('',(#10716,#10717,#10718,#10719));
#2845=EDGE_LOOP('',(#10720,#10721,#10722,#10723));
#2846=EDGE_LOOP('',(#10724,#10725,#10726,#10727));
#2847=EDGE_LOOP('',(#10728,#10729,#10730,#10731));
#2848=EDGE_LOOP('',(#10732,#10733,#10734,#10735));
#2849=EDGE_LOOP('',(#10736,#10737,#10738,#10739));
#2850=EDGE_LOOP('',(#10740,#10741,#10742,#10743));
#2851=EDGE_LOOP('',(#10744,#10745,#10746,#10747));
#2852=EDGE_LOOP('',(#10748,#10749,#10750,#10751));
#2853=EDGE_LOOP('',(#10752,#10753,#10754,#10755));
#2854=EDGE_LOOP('',(#10756,#10757,#10758,#10759));
#2855=EDGE_LOOP('',(#10760,#10761,#10762,#10763));
#2856=EDGE_LOOP('',(#10764,#10765,#10766,#10767));
#2857=EDGE_LOOP('',(#10768,#10769,#10770,#10771));
#2858=EDGE_LOOP('',(#10772,#10773,#10774,#10775));
#2859=EDGE_LOOP('',(#10776,#10777,#10778,#10779));
#2860=EDGE_LOOP('',(#10780,#10781,#10782,#10783));
#2861=EDGE_LOOP('',(#10784,#10785,#10786,#10787));
#2862=EDGE_LOOP('',(#10788,#10789,#10790,#10791));
#2863=EDGE_LOOP('',(#10792,#10793,#10794,#10795));
#2864=EDGE_LOOP('',(#10796,#10797,#10798,#10799));
#2865=EDGE_LOOP('',(#10800,#10801,#10802,#10803));
#2866=EDGE_LOOP('',(#10804,#10805,#10806,#10807));
#2867=EDGE_LOOP('',(#10808,#10809,#10810,#10811));
#2868=EDGE_LOOP('',(#10812,#10813,#10814,#10815));
#2869=EDGE_LOOP('',(#10816,#10817,#10818,#10819));
#2870=EDGE_LOOP('',(#10820,#10821,#10822,#10823));
#2871=EDGE_LOOP('',(#10824,#10825,#10826,#10827));
#2872=EDGE_LOOP('',(#10828,#10829,#10830,#10831));
#2873=EDGE_LOOP('',(#10832,#10833,#10834,#10835));
#2874=EDGE_LOOP('',(#10836,#10837,#10838,#10839));
#2875=EDGE_LOOP('',(#10840,#10841,#10842,#10843));
#2876=EDGE_LOOP('',(#10844,#10845,#10846,#10847));
#2877=EDGE_LOOP('',(#10848,#10849,#10850,#10851));
#2878=EDGE_LOOP('',(#10852,#10853,#10854,#10855));
#2879=EDGE_LOOP('',(#10856,#10857,#10858,#10859));
#2880=EDGE_LOOP('',(#10860,#10861,#10862,#10863));
#2881=EDGE_LOOP('',(#10864,#10865,#10866,#10867));
#2882=EDGE_LOOP('',(#10868,#10869,#10870,#10871));
#2883=EDGE_LOOP('',(#10872,#10873,#10874,#10875));
#2884=EDGE_LOOP('',(#10876,#10877,#10878,#10879));
#2885=EDGE_LOOP('',(#10880,#10881,#10882,#10883));
#2886=EDGE_LOOP('',(#10884,#10885,#10886,#10887));
#2887=EDGE_LOOP('',(#10888,#10889,#10890,#10891));
#2888=EDGE_LOOP('',(#10892,#10893,#10894,#10895));
#2889=EDGE_LOOP('',(#10896,#10897,#10898,#10899));
#2890=EDGE_LOOP('',(#10900,#10901,#10902,#10903));
#2891=EDGE_LOOP('',(#10904,#10905,#10906,#10907));
#2892=EDGE_LOOP('',(#10908,#10909,#10910,#10911));
#2893=EDGE_LOOP('',(#10912,#10913,#10914,#10915));
#2894=EDGE_LOOP('',(#10916,#10917,#10918,#10919));
#2895=EDGE_LOOP('',(#10920,#10921,#10922,#10923));
#2896=EDGE_LOOP('',(#10924,#10925,#10926,#10927));
#2897=EDGE_LOOP('',(#10928,#10929,#10930,#10931));
#2898=EDGE_LOOP('',(#10932,#10933,#10934,#10935));
#2899=EDGE_LOOP('',(#10936,#10937,#10938,#10939));
#2900=EDGE_LOOP('',(#10940,#10941,#10942,#10943));
#2901=EDGE_LOOP('',(#10944,#10945,#10946,#10947));
#2902=EDGE_LOOP('',(#10948,#10949,#10950,#10951));
#2903=EDGE_LOOP('',(#10952,#10953,#10954,#10955));
#2904=EDGE_LOOP('',(#10956));
#2905=EDGE_LOOP('',(#10957,#10958,#10959,#10960));
#2906=EDGE_LOOP('',(#10961,#10962,#10963,#10964));
#2907=EDGE_LOOP('',(#10965,#10966,#10967,#10968));
#2908=EDGE_LOOP('',(#10969));
#2909=EDGE_LOOP('',(#10970));
#2910=EDGE_LOOP('',(#10971,#10972,#10973,#10974));
#2911=EDGE_LOOP('',(#10975,#10976,#10977,#10978));
#2912=EDGE_LOOP('',(#10979,#10980,#10981,#10982));
#2913=EDGE_LOOP('',(#10983));
#2914=EDGE_LOOP('',(#10984,#10985,#10986,#10987));
#2915=EDGE_LOOP('',(#10988,#10989,#10990,#10991));
#2916=EDGE_LOOP('',(#10992,#10993,#10994,#10995));
#2917=EDGE_LOOP('',(#10996,#10997,#10998,#10999));
#2918=EDGE_LOOP('',(#11000,#11001,#11002,#11003));
#2919=EDGE_LOOP('',(#11004,#11005,#11006,#11007));
#2920=EDGE_LOOP('',(#11008,#11009,#11010,#11011,#11012,#11013));
#2921=EDGE_LOOP('',(#11014,#11015,#11016,#11017,#11018,#11019));
#2922=EDGE_LOOP('',(#11020,#11021,#11022,#11023));
#2923=EDGE_LOOP('',(#11024));
#2924=EDGE_LOOP('',(#11025));
#2925=EDGE_LOOP('',(#11026));
#2926=EDGE_LOOP('',(#11027));
#2927=EDGE_LOOP('',(#11028));
#2928=EDGE_LOOP('',(#11029,#11030,#11031,#11032));
#2929=EDGE_LOOP('',(#11033,#11034,#11035,#11036));
#2930=EDGE_LOOP('',(#11037));
#2931=EDGE_LOOP('',(#11038));
#2932=EDGE_LOOP('',(#11039));
#2933=EDGE_LOOP('',(#11040));
#2934=EDGE_LOOP('',(#11041,#11042,#11043,#11044));
#2935=EDGE_LOOP('',(#11045,#11046,#11047,#11048));
#2936=EDGE_LOOP('',(#11049));
#2937=EDGE_LOOP('',(#11050));
#2938=EDGE_LOOP('',(#11051,#11052,#11053,#11054));
#2939=EDGE_LOOP('',(#11055));
#2940=EDGE_LOOP('',(#11056));
#2941=EDGE_LOOP('',(#11057,#11058,#11059,#11060));
#2942=EDGE_LOOP('',(#11061,#11062,#11063,#11064));
#2943=EDGE_LOOP('',(#11065));
#2944=EDGE_LOOP('',(#11066));
#2945=EDGE_LOOP('',(#11067));
#2946=EDGE_LOOP('',(#11068,#11069));
#2947=EDGE_LOOP('',(#11070,#11071,#11072,#11073,#11074,#11075,#11076,#11077,
#11078,#11079,#11080));
#2948=EDGE_LOOP('',(#11081,#11082));
#2949=EDGE_LOOP('',(#11083,#11084,#11085,#11086,#11087,#11088,#11089,#11090,
#11091,#11092,#11093,#11094));
#2950=EDGE_LOOP('',(#11095,#11096,#11097,#11098,#11099,#11100,#11101,#11102,
#11103));
#2951=EDGE_LOOP('',(#11104));
#2952=EDGE_LOOP('',(#11105));
#2953=EDGE_LOOP('',(#11106));
#2954=EDGE_LOOP('',(#11107));
#2955=EDGE_LOOP('',(#11108,#11109,#11110,#11111));
#2956=EDGE_LOOP('',(#11112,#11113,#11114,#11115));
#2957=EDGE_LOOP('',(#11116,#11117,#11118,#11119));
#2958=EDGE_LOOP('',(#11120,#11121,#11122,#11123));
#2959=EDGE_LOOP('',(#11124,#11125,#11126,#11127));
#2960=EDGE_LOOP('',(#11128,#11129,#11130,#11131));
#2961=EDGE_LOOP('',(#11132,#11133,#11134,#11135,#11136,#11137));
#2962=EDGE_LOOP('',(#11138));
#2963=EDGE_LOOP('',(#11139,#11140,#11141,#11142,#11143,#11144));
#2964=EDGE_LOOP('',(#11145,#11146,#11147,#11148));
#2965=EDGE_LOOP('',(#11149,#11150,#11151,#11152));
#2966=EDGE_LOOP('',(#11153,#11154,#11155,#11156));
#2967=EDGE_LOOP('',(#11157));
#2968=LINE('',#18557,#3719);
#2969=LINE('',#18564,#3720);
#2970=LINE('',#18571,#3721);
#2971=LINE('',#18578,#3722);
#2972=LINE('',#18585,#3723);
#2973=LINE('',#18592,#3724);
#2974=LINE('',#18599,#3725);
#2975=LINE('',#18606,#3726);
#2976=LINE('',#18613,#3727);
#2977=LINE('',#18620,#3728);
#2978=LINE('',#18627,#3729);
#2979=LINE('',#18634,#3730);
#2980=LINE('',#18641,#3731);
#2981=LINE('',#18648,#3732);
#2982=LINE('',#18654,#3733);
#2983=LINE('',#18656,#3734);
#2984=LINE('',#18658,#3735);
#2985=LINE('',#18659,#3736);
#2986=LINE('',#18662,#3737);
#2987=LINE('',#18664,#3738);
#2988=LINE('',#18665,#3739);
#2989=LINE('',#18668,#3740);
#2990=LINE('',#18670,#3741);
#2991=LINE('',#18671,#3742);
#2992=LINE('',#18673,#3743);
#2993=LINE('',#18674,#3744);
#2994=LINE('',#18681,#3745);
#2995=LINE('',#18683,#3746);
#2996=LINE('',#18685,#3747);
#2997=LINE('',#18686,#3748);
#2998=LINE('',#18689,#3749);
#2999=LINE('',#18691,#3750);
#3000=LINE('',#18692,#3751);
#3001=LINE('',#18695,#3752);
#3002=LINE('',#18697,#3753);
#3003=LINE('',#18698,#3754);
#3004=LINE('',#18700,#3755);
#3005=LINE('',#18701,#3756);
#3006=LINE('',#18708,#3757);
#3007=LINE('',#18710,#3758);
#3008=LINE('',#18712,#3759);
#3009=LINE('',#18713,#3760);
#3010=LINE('',#18716,#3761);
#3011=LINE('',#18718,#3762);
#3012=LINE('',#18719,#3763);
#3013=LINE('',#18722,#3764);
#3014=LINE('',#18724,#3765);
#3015=LINE('',#18725,#3766);
#3016=LINE('',#18727,#3767);
#3017=LINE('',#18728,#3768);
#3018=LINE('',#18736,#3769);
#3019=LINE('',#18742,#3770);
#3020=LINE('',#18748,#3771);
#3021=LINE('',#18754,#3772);
#3022=LINE('',#18760,#3773);
#3023=LINE('',#18766,#3774);
#3024=LINE('',#18772,#3775);
#3025=LINE('',#18778,#3776);
#3026=LINE('',#18784,#3777);
#3027=LINE('',#18789,#3778);
#3028=LINE('',#18791,#3779);
#3029=LINE('',#18793,#3780);
#3030=LINE('',#18794,#3781);
#3031=LINE('',#18798,#3782);
#3032=LINE('',#18800,#3783);
#3033=LINE('',#18802,#3784);
#3034=LINE('',#18803,#3785);
#3035=LINE('',#18806,#3786);
#3036=LINE('',#18808,#3787);
#3037=LINE('',#18809,#3788);
#3038=LINE('',#18812,#3789);
#3039=LINE('',#18814,#3790);
#3040=LINE('',#18815,#3791);
#3041=LINE('',#18818,#3792);
#3042=LINE('',#18820,#3793);
#3043=LINE('',#18821,#3794);
#3044=LINE('',#18822,#3795);
#3045=LINE('',#18825,#3796);
#3046=LINE('',#18826,#3797);
#3047=LINE('',#18829,#3798);
#3048=LINE('',#18830,#3799);
#3049=LINE('',#18831,#3800);
#3050=LINE('',#18833,#3801);
#3051=LINE('',#18841,#3802);
#3052=LINE('',#18847,#3803);
#3053=LINE('',#18855,#3804);
#3054=LINE('',#18859,#3805);
#3055=LINE('',#18864,#3806);
#3056=LINE('',#18868,#3807);
#3057=LINE('',#18873,#3808);
#3058=LINE('',#18877,#3809);
#3059=LINE('',#18882,#3810);
#3060=LINE('',#18886,#3811);
#3061=LINE('',#18907,#3812);
#3062=LINE('',#18913,#3813);
#3063=LINE('',#18919,#3814);
#3064=LINE('',#18923,#3815);
#3065=LINE('',#18928,#3816);
#3066=LINE('',#18932,#3817);
#3067=LINE('',#18937,#3818);
#3068=LINE('',#18941,#3819);
#3069=LINE('',#18946,#3820);
#3070=LINE('',#18950,#3821);
#3071=LINE('',#18969,#3822);
#3072=LINE('',#18977,#3823);
#3073=LINE('',#18984,#3824);
#3074=LINE('',#18993,#3825);
#3075=LINE('',#19001,#3826);
#3076=LINE('',#19005,#3827);
#3077=LINE('',#19010,#3828);
#3078=LINE('',#19015,#3829);
#3079=LINE('',#19017,#3830);
#3080=LINE('',#19019,#3831);
#3081=LINE('',#19020,#3832);
#3082=LINE('',#19023,#3833);
#3083=LINE('',#19025,#3834);
#3084=LINE('',#19026,#3835);
#3085=LINE('',#19029,#3836);
#3086=LINE('',#19031,#3837);
#3087=LINE('',#19032,#3838);
#3088=LINE('',#19034,#3839);
#3089=LINE('',#19035,#3840);
#3090=LINE('',#19043,#3841);
#3091=LINE('',#19049,#3842);
#3092=LINE('',#19058,#3843);
#3093=LINE('',#19067,#3844);
#3094=LINE('',#19075,#3845);
#3095=LINE('',#19079,#3846);
#3096=LINE('',#19084,#3847);
#3097=LINE('',#19089,#3848);
#3098=LINE('',#19091,#3849);
#3099=LINE('',#19093,#3850);
#3100=LINE('',#19094,#3851);
#3101=LINE('',#19097,#3852);
#3102=LINE('',#19099,#3853);
#3103=LINE('',#19100,#3854);
#3104=LINE('',#19103,#3855);
#3105=LINE('',#19105,#3856);
#3106=LINE('',#19106,#3857);
#3107=LINE('',#19108,#3858);
#3108=LINE('',#19109,#3859);
#3109=LINE('',#19117,#3860);
#3110=LINE('',#19123,#3861);
#3111=LINE('',#19132,#3862);
#3112=LINE('',#19138,#3863);
#3113=LINE('',#19146,#3864);
#3114=LINE('',#19150,#3865);
#3115=LINE('',#19162,#3866);
#3116=LINE('',#19166,#3867);
#3117=LINE('',#19210,#3868);
#3118=LINE('',#19250,#3869);
#3119=LINE('',#19257,#3870);
#3120=LINE('',#19259,#3871);
#3121=LINE('',#19260,#3872);
#3122=LINE('',#19263,#3873);
#3123=LINE('',#19265,#3874);
#3124=LINE('',#19266,#3875);
#3125=LINE('',#19269,#3876);
#3126=LINE('',#19271,#3877);
#3127=LINE('',#19272,#3878);
#3128=LINE('',#19276,#3879);
#3129=LINE('',#19280,#3880);
#3130=LINE('',#19283,#3881);
#3131=LINE('',#19288,#3882);
#3132=LINE('',#19290,#3883);
#3133=LINE('',#19292,#3884);
#3134=LINE('',#19293,#3885);
#3135=LINE('',#19295,#3886);
#3136=LINE('',#19298,#3887);
#3137=LINE('',#19299,#3888);
#3138=LINE('',#19302,#3889);
#3139=LINE('',#19303,#3890);
#3140=LINE('',#19305,#3891);
#3141=LINE('',#19312,#3892);
#3142=LINE('',#19321,#3893);
#3143=LINE('',#19330,#3894);
#3144=LINE('',#19339,#3895);
#3145=LINE('',#19347,#3896);
#3146=LINE('',#19351,#3897);
#3147=LINE('',#19355,#3898);
#3148=LINE('',#19359,#3899);
#3149=LINE('',#19363,#3900);
#3150=LINE('',#19365,#3901);
#3151=LINE('',#19367,#3902);
#3152=LINE('',#19368,#3903);
#3153=LINE('',#19371,#3904);
#3154=LINE('',#19373,#3905);
#3155=LINE('',#19374,#3906);
#3156=LINE('',#19377,#3907);
#3157=LINE('',#19379,#3908);
#3158=LINE('',#19380,#3909);
#3159=LINE('',#19383,#3910);
#3160=LINE('',#19385,#3911);
#3161=LINE('',#19386,#3912);
#3162=LINE('',#19389,#3913);
#3163=LINE('',#19391,#3914);
#3164=LINE('',#19392,#3915);
#3165=LINE('',#19395,#3916);
#3166=LINE('',#19397,#3917);
#3167=LINE('',#19398,#3918);
#3168=LINE('',#19401,#3919);
#3169=LINE('',#19403,#3920);
#3170=LINE('',#19404,#3921);
#3171=LINE('',#19407,#3922);
#3172=LINE('',#19409,#3923);
#3173=LINE('',#19410,#3924);
#3174=LINE('',#19413,#3925);
#3175=LINE('',#19415,#3926);
#3176=LINE('',#19416,#3927);
#3177=LINE('',#19419,#3928);
#3178=LINE('',#19421,#3929);
#3179=LINE('',#19422,#3930);
#3180=LINE('',#19425,#3931);
#3181=LINE('',#19427,#3932);
#3182=LINE('',#19428,#3933);
#3183=LINE('',#19430,#3934);
#3184=LINE('',#19431,#3935);
#3185=LINE('',#19448,#3936);
#3186=LINE('',#19454,#3937);
#3187=LINE('',#19458,#3938);
#3188=LINE('',#19464,#3939);
#3189=LINE('',#19469,#3940);
#3190=LINE('',#19484,#3941);
#3191=LINE('',#19493,#3942);
#3192=LINE('',#19497,#3943);
#3193=LINE('',#19501,#3944);
#3194=LINE('',#19504,#3945);
#3195=LINE('',#19657,#3946);
#3196=LINE('',#19953,#3947);
#3197=LINE('',#19995,#3948);
#3198=LINE('',#20000,#3949);
#3199=LINE('',#20009,#3950);
#3200=LINE('',#20014,#3951);
#3201=LINE('',#20026,#3952);
#3202=LINE('',#20032,#3953);
#3203=LINE('',#20038,#3954);
#3204=LINE('',#20044,#3955);
#3205=LINE('',#20050,#3956);
#3206=LINE('',#20056,#3957);
#3207=LINE('',#20062,#3958);
#3208=LINE('',#20068,#3959);
#3209=LINE('',#20074,#3960);
#3210=LINE('',#20080,#3961);
#3211=LINE('',#20085,#3962);
#3212=LINE('',#20087,#3963);
#3213=LINE('',#20089,#3964);
#3214=LINE('',#20090,#3965);
#3215=LINE('',#20093,#3966);
#3216=LINE('',#20095,#3967);
#3217=LINE('',#20096,#3968);
#3218=LINE('',#20099,#3969);
#3219=LINE('',#20101,#3970);
#3220=LINE('',#20102,#3971);
#3221=LINE('',#20104,#3972);
#3222=LINE('',#20105,#3973);
#3223=LINE('',#20113,#3974);
#3224=LINE('',#20119,#3975);
#3225=LINE('',#20125,#3976);
#3226=LINE('',#20131,#3977);
#3227=LINE('',#20137,#3978);
#3228=LINE('',#20142,#3979);
#3229=LINE('',#20146,#3980);
#3230=LINE('',#20149,#3981);
#3231=LINE('',#20153,#3982);
#3232=LINE('',#20157,#3983);
#3233=LINE('',#20160,#3984);
#3234=LINE('',#20164,#3985);
#3235=LINE('',#20168,#3986);
#3236=LINE('',#20171,#3987);
#3237=LINE('',#20175,#3988);
#3238=LINE('',#20179,#3989);
#3239=LINE('',#20182,#3990);
#3240=LINE('',#20185,#3991);
#3241=LINE('',#20187,#3992);
#3242=LINE('',#20189,#3993);
#3243=LINE('',#20191,#3994);
#3244=LINE('',#20193,#3995);
#3245=LINE('',#20195,#3996);
#3246=LINE('',#20197,#3997);
#3247=LINE('',#20199,#3998);
#3248=LINE('',#20200,#3999);
#3249=LINE('',#20201,#4000);
#3250=LINE('',#20204,#4001);
#3251=LINE('',#20206,#4002);
#3252=LINE('',#20208,#4003);
#3253=LINE('',#20210,#4004);
#3254=LINE('',#20212,#4005);
#3255=LINE('',#20214,#4006);
#3256=LINE('',#20216,#4007);
#3257=LINE('',#20218,#4008);
#3258=LINE('',#20219,#4009);
#3259=LINE('',#20220,#4010);
#3260=LINE('',#20225,#4011);
#3261=LINE('',#20231,#4012);
#3262=LINE('',#20237,#4013);
#3263=LINE('',#20243,#4014);
#3264=LINE('',#20246,#4015);
#3265=LINE('',#20247,#4016);
#3266=LINE('',#20249,#4017);
#3267=LINE('',#20250,#4018);
#3268=LINE('',#20252,#4019);
#3269=LINE('',#20254,#4020);
#3270=LINE('',#20256,#4021);
#3271=LINE('',#20258,#4022);
#3272=LINE('',#20266,#4023);
#3273=LINE('',#20272,#4024);
#3274=LINE('',#20280,#4025);
#3275=LINE('',#20284,#4026);
#3276=LINE('',#20289,#4027);
#3277=LINE('',#20293,#4028);
#3278=LINE('',#20298,#4029);
#3279=LINE('',#20302,#4030);
#3280=LINE('',#20307,#4031);
#3281=LINE('',#20311,#4032);
#3282=LINE('',#20332,#4033);
#3283=LINE('',#20338,#4034);
#3284=LINE('',#20344,#4035);
#3285=LINE('',#20348,#4036);
#3286=LINE('',#20353,#4037);
#3287=LINE('',#20357,#4038);
#3288=LINE('',#20362,#4039);
#3289=LINE('',#20366,#4040);
#3290=LINE('',#20371,#4041);
#3291=LINE('',#20375,#4042);
#3292=LINE('',#20394,#4043);
#3293=LINE('',#20402,#4044);
#3294=LINE('',#20409,#4045);
#3295=LINE('',#20416,#4046);
#3296=LINE('',#20423,#4047);
#3297=LINE('',#20428,#4048);
#3298=LINE('',#20430,#4049);
#3299=LINE('',#20432,#4050);
#3300=LINE('',#20433,#4051);
#3301=LINE('',#20436,#4052);
#3302=LINE('',#20438,#4053);
#3303=LINE('',#20439,#4054);
#3304=LINE('',#20442,#4055);
#3305=LINE('',#20444,#4056);
#3306=LINE('',#20445,#4057);
#3307=LINE('',#20447,#4058);
#3308=LINE('',#20448,#4059);
#3309=LINE('',#20457,#4060);
#3310=LINE('',#20464,#4061);
#3311=LINE('',#20497,#4062);
#3312=LINE('',#20500,#4063);
#3313=LINE('',#20504,#4064);
#3314=LINE('',#20506,#4065);
#3315=LINE('',#20511,#4066);
#3316=LINE('',#20513,#4067);
#3317=LINE('',#20515,#4068);
#3318=LINE('',#20516,#4069);
#3319=LINE('',#20519,#4070);
#3320=LINE('',#20521,#4071);
#3321=LINE('',#20522,#4072);
#3322=LINE('',#20525,#4073);
#3323=LINE('',#20527,#4074);
#3324=LINE('',#20528,#4075);
#3325=LINE('',#20530,#4076);
#3326=LINE('',#20531,#4077);
#3327=LINE('',#20539,#4078);
#3328=LINE('',#20543,#4079);
#3329=LINE('',#20547,#4080);
#3330=LINE('',#20551,#4081);
#3331=LINE('',#20555,#4082);
#3332=LINE('',#20559,#4083);
#3333=LINE('',#20563,#4084);
#3334=LINE('',#20567,#4085);
#3335=LINE('',#20571,#4086);
#3336=LINE('',#20575,#4087);
#3337=LINE('',#20579,#4088);
#3338=LINE('',#20583,#4089);
#3339=LINE('',#20587,#4090);
#3340=LINE('',#20591,#4091);
#3341=LINE('',#20595,#4092);
#3342=LINE('',#20599,#4093);
#3343=LINE('',#20601,#4094);
#3344=LINE('',#20603,#4095);
#3345=LINE('',#20605,#4096);
#3346=LINE('',#20607,#4097);
#3347=LINE('',#20609,#4098);
#3348=LINE('',#20610,#4099);
#3349=LINE('',#20612,#4100);
#3350=LINE('',#20614,#4101);
#3351=LINE('',#20616,#4102);
#3352=LINE('',#20618,#4103);
#3353=LINE('',#20620,#4104);
#3354=LINE('',#20621,#4105);
#3355=LINE('',#20624,#4106);
#3356=LINE('',#20626,#4107);
#3357=LINE('',#20628,#4108);
#3358=LINE('',#20630,#4109);
#3359=LINE('',#20631,#4110);
#3360=LINE('',#20633,#4111);
#3361=LINE('',#20635,#4112);
#3362=LINE('',#20637,#4113);
#3363=LINE('',#20639,#4114);
#3364=LINE('',#20640,#4115);
#3365=LINE('',#20643,#4116);
#3366=LINE('',#20644,#4117);
#3367=LINE('',#20647,#4118);
#3368=LINE('',#20648,#4119);
#3369=LINE('',#20651,#4120);
#3370=LINE('',#20652,#4121);
#3371=LINE('',#20655,#4122);
#3372=LINE('',#20656,#4123);
#3373=LINE('',#20658,#4124);
#3374=LINE('',#20661,#4125);
#3375=LINE('',#20662,#4126);
#3376=LINE('',#20665,#4127);
#3377=LINE('',#20666,#4128);
#3378=LINE('',#20669,#4129);
#3379=LINE('',#20670,#4130);
#3380=LINE('',#20673,#4131);
#3381=LINE('',#20674,#4132);
#3382=LINE('',#20676,#4133);
#3383=LINE('',#20682,#4134);
#3384=LINE('',#20684,#4135);
#3385=LINE('',#20686,#4136);
#3386=LINE('',#20687,#4137);
#3387=LINE('',#20690,#4138);
#3388=LINE('',#20692,#4139);
#3389=LINE('',#20693,#4140);
#3390=LINE('',#20696,#4141);
#3391=LINE('',#20698,#4142);
#3392=LINE('',#20699,#4143);
#3393=LINE('',#20702,#4144);
#3394=LINE('',#20704,#4145);
#3395=LINE('',#20705,#4146);
#3396=LINE('',#20708,#4147);
#3397=LINE('',#20710,#4148);
#3398=LINE('',#20711,#4149);
#3399=LINE('',#20714,#4150);
#3400=LINE('',#20716,#4151);
#3401=LINE('',#20717,#4152);
#3402=LINE('',#20720,#4153);
#3403=LINE('',#20722,#4154);
#3404=LINE('',#20723,#4155);
#3405=LINE('',#20725,#4156);
#3406=LINE('',#20726,#4157);
#3407=LINE('',#20733,#4158);
#3408=LINE('',#20735,#4159);
#3409=LINE('',#20737,#4160);
#3410=LINE('',#20738,#4161);
#3411=LINE('',#20741,#4162);
#3412=LINE('',#20743,#4163);
#3413=LINE('',#20744,#4164);
#3414=LINE('',#20747,#4165);
#3415=LINE('',#20749,#4166);
#3416=LINE('',#20750,#4167);
#3417=LINE('',#20753,#4168);
#3418=LINE('',#20755,#4169);
#3419=LINE('',#20756,#4170);
#3420=LINE('',#20759,#4171);
#3421=LINE('',#20761,#4172);
#3422=LINE('',#20762,#4173);
#3423=LINE('',#20765,#4174);
#3424=LINE('',#20767,#4175);
#3425=LINE('',#20768,#4176);
#3426=LINE('',#20771,#4177);
#3427=LINE('',#20773,#4178);
#3428=LINE('',#20774,#4179);
#3429=LINE('',#20776,#4180);
#3430=LINE('',#20777,#4181);
#3431=LINE('',#20787,#4182);
#3432=LINE('',#20789,#4183);
#3433=LINE('',#20791,#4184);
#3434=LINE('',#20792,#4185);
#3435=LINE('',#20795,#4186);
#3436=LINE('',#20797,#4187);
#3437=LINE('',#20798,#4188);
#3438=LINE('',#20801,#4189);
#3439=LINE('',#20803,#4190);
#3440=LINE('',#20804,#4191);
#3441=LINE('',#20807,#4192);
#3442=LINE('',#20809,#4193);
#3443=LINE('',#20810,#4194);
#3444=LINE('',#20813,#4195);
#3445=LINE('',#20815,#4196);
#3446=LINE('',#20816,#4197);
#3447=LINE('',#20818,#4198);
#3448=LINE('',#20819,#4199);
#3449=LINE('',#20831,#4200);
#3450=LINE('',#20835,#4201);
#3451=LINE('',#20839,#4202);
#3452=LINE('',#20846,#4203);
#3453=LINE('',#20848,#4204);
#3454=LINE('',#20863,#4205);
#3455=LINE('',#20869,#4206);
#3456=LINE('',#20873,#4207);
#3457=LINE('',#20879,#4208);
#3458=LINE('',#20884,#4209);
#3459=LINE('',#20899,#4210);
#3460=LINE('',#20908,#4211);
#3461=LINE('',#20912,#4212);
#3462=LINE('',#20916,#4213);
#3463=LINE('',#20919,#4214);
#3464=LINE('',#21055,#4215);
#3465=LINE('',#21308,#4216);
#3466=LINE('',#21350,#4217);
#3467=LINE('',#21355,#4218);
#3468=LINE('',#21364,#4219);
#3469=LINE('',#21369,#4220);
#3470=LINE('',#21379,#4221);
#3471=LINE('',#21381,#4222);
#3472=LINE('',#21383,#4223);
#3473=LINE('',#21384,#4224);
#3474=LINE('',#21387,#4225);
#3475=LINE('',#21389,#4226);
#3476=LINE('',#21390,#4227);
#3477=LINE('',#21393,#4228);
#3478=LINE('',#21395,#4229);
#3479=LINE('',#21396,#4230);
#3480=LINE('',#21399,#4231);
#3481=LINE('',#21401,#4232);
#3482=LINE('',#21402,#4233);
#3483=LINE('',#21405,#4234);
#3484=LINE('',#21407,#4235);
#3485=LINE('',#21408,#4236);
#3486=LINE('',#21410,#4237);
#3487=LINE('',#21411,#4238);
#3488=LINE('',#21423,#4239);
#3489=LINE('',#21427,#4240);
#3490=LINE('',#21431,#4241);
#3491=LINE('',#21438,#4242);
#3492=LINE('',#21440,#4243);
#3493=LINE('',#21447,#4244);
#3494=LINE('',#21461,#4245);
#3495=LINE('',#21464,#4246);
#3496=LINE('',#21470,#4247);
#3497=LINE('',#21476,#4248);
#3498=LINE('',#21484,#4249);
#3499=LINE('',#21491,#4250);
#3500=LINE('',#21497,#4251);
#3501=LINE('',#21506,#4252);
#3502=LINE('',#21512,#4253);
#3503=LINE('',#21521,#4254);
#3504=LINE('',#21530,#4255);
#3505=LINE('',#21539,#4256);
#3506=LINE('',#21545,#4257);
#3507=LINE('',#21593,#4258);
#3508=LINE('',#21677,#4259);
#3509=LINE('',#21721,#4260);
#3510=LINE('',#21723,#4261);
#3511=LINE('',#21809,#4262);
#3512=LINE('',#21886,#4263);
#3513=LINE('',#21890,#4264);
#3514=LINE('',#21892,#4265);
#3515=LINE('',#21981,#4266);
#3516=LINE('',#22069,#4267);
#3517=LINE('',#22072,#4268);
#3518=LINE('',#22073,#4269);
#3519=LINE('',#22075,#4270);
#3520=LINE('',#22077,#4271);
#3521=LINE('',#22079,#4272);
#3522=LINE('',#22081,#4273);
#3523=LINE('',#22083,#4274);
#3524=LINE('',#22085,#4275);
#3525=LINE('',#22087,#4276);
#3526=LINE('',#22089,#4277);
#3527=LINE('',#22091,#4278);
#3528=LINE('',#22093,#4279);
#3529=LINE('',#22095,#4280);
#3530=LINE('',#22097,#4281);
#3531=LINE('',#22099,#4282);
#3532=LINE('',#22101,#4283);
#3533=LINE('',#22103,#4284);
#3534=LINE('',#22105,#4285);
#3535=LINE('',#22107,#4286);
#3536=LINE('',#22109,#4287);
#3537=LINE('',#22111,#4288);
#3538=LINE('',#22113,#4289);
#3539=LINE('',#22115,#4290);
#3540=LINE('',#22117,#4291);
#3541=LINE('',#22119,#4292);
#3542=LINE('',#22121,#4293);
#3543=LINE('',#22123,#4294);
#3544=LINE('',#22125,#4295);
#3545=LINE('',#22127,#4296);
#3546=LINE('',#22129,#4297);
#3547=LINE('',#22131,#4298);
#3548=LINE('',#22133,#4299);
#3549=LINE('',#22135,#4300);
#3550=LINE('',#22137,#4301);
#3551=LINE('',#22139,#4302);
#3552=LINE('',#22141,#4303);
#3553=LINE('',#22143,#4304);
#3554=LINE('',#22145,#4305);
#3555=LINE('',#22147,#4306);
#3556=LINE('',#22149,#4307);
#3557=LINE('',#22157,#4308);
#3558=LINE('',#22171,#4309);
#3559=LINE('',#22174,#4310);
#3560=LINE('',#22180,#4311);
#3561=LINE('',#22187,#4312);
#3562=LINE('',#22193,#4313);
#3563=LINE('',#22202,#4314);
#3564=LINE('',#22208,#4315);
#3565=LINE('',#22217,#4316);
#3566=LINE('',#22226,#4317);
#3567=LINE('',#22235,#4318);
#3568=LINE('',#22241,#4319);
#3569=LINE('',#22289,#4320);
#3570=LINE('',#22373,#4321);
#3571=LINE('',#22417,#4322);
#3572=LINE('',#22419,#4323);
#3573=LINE('',#22505,#4324);
#3574=LINE('',#22582,#4325);
#3575=LINE('',#22586,#4326);
#3576=LINE('',#22588,#4327);
#3577=LINE('',#22757,#4328);
#3578=LINE('',#22925,#4329);
#3579=LINE('',#22928,#4330);
#3580=LINE('',#22929,#4331);
#3581=LINE('',#22931,#4332);
#3582=LINE('',#22933,#4333);
#3583=LINE('',#22935,#4334);
#3584=LINE('',#22937,#4335);
#3585=LINE('',#22939,#4336);
#3586=LINE('',#22941,#4337);
#3587=LINE('',#22943,#4338);
#3588=LINE('',#22945,#4339);
#3589=LINE('',#22947,#4340);
#3590=LINE('',#22949,#4341);
#3591=LINE('',#22951,#4342);
#3592=LINE('',#22953,#4343);
#3593=LINE('',#22955,#4344);
#3594=LINE('',#22957,#4345);
#3595=LINE('',#22959,#4346);
#3596=LINE('',#22961,#4347);
#3597=LINE('',#22963,#4348);
#3598=LINE('',#22965,#4349);
#3599=LINE('',#22967,#4350);
#3600=LINE('',#22969,#4351);
#3601=LINE('',#22971,#4352);
#3602=LINE('',#22973,#4353);
#3603=LINE('',#22975,#4354);
#3604=LINE('',#22977,#4355);
#3605=LINE('',#22979,#4356);
#3606=LINE('',#22981,#4357);
#3607=LINE('',#22983,#4358);
#3608=LINE('',#22985,#4359);
#3609=LINE('',#22987,#4360);
#3610=LINE('',#22989,#4361);
#3611=LINE('',#22991,#4362);
#3612=LINE('',#22993,#4363);
#3613=LINE('',#22995,#4364);
#3614=LINE('',#22997,#4365);
#3615=LINE('',#22999,#4366);
#3616=LINE('',#23001,#4367);
#3617=LINE('',#23003,#4368);
#3618=LINE('',#23005,#4369);
#3619=LINE('',#23007,#4370);
#3620=LINE('',#23009,#4371);
#3621=LINE('',#23011,#4372);
#3622=LINE('',#23013,#4373);
#3623=LINE('',#23015,#4374);
#3624=LINE('',#23017,#4375);
#3625=LINE('',#23019,#4376);
#3626=LINE('',#23021,#4377);
#3627=LINE('',#23023,#4378);
#3628=LINE('',#23025,#4379);
#3629=LINE('',#23027,#4380);
#3630=LINE('',#23029,#4381);
#3631=LINE('',#23031,#4382);
#3632=LINE('',#23033,#4383);
#3633=LINE('',#23035,#4384);
#3634=LINE('',#23037,#4385);
#3635=LINE('',#23039,#4386);
#3636=LINE('',#23041,#4387);
#3637=LINE('',#23043,#4388);
#3638=LINE('',#23045,#4389);
#3639=LINE('',#23047,#4390);
#3640=LINE('',#23049,#4391);
#3641=LINE('',#23051,#4392);
#3642=LINE('',#23053,#4393);
#3643=LINE('',#23055,#4394);
#3644=LINE('',#23057,#4395);
#3645=LINE('',#23059,#4396);
#3646=LINE('',#23061,#4397);
#3647=LINE('',#23063,#4398);
#3648=LINE('',#23065,#4399);
#3649=LINE('',#23067,#4400);
#3650=LINE('',#23069,#4401);
#3651=LINE('',#23071,#4402);
#3652=LINE('',#23073,#4403);
#3653=LINE('',#23075,#4404);
#3654=LINE('',#23077,#4405);
#3655=LINE('',#23079,#4406);
#3656=LINE('',#23081,#4407);
#3657=LINE('',#23083,#4408);
#3658=LINE('',#23085,#4409);
#3659=LINE('',#23094,#4410);
#3660=LINE('',#23098,#4411);
#3661=LINE('',#23102,#4412);
#3662=LINE('',#23109,#4413);
#3663=LINE('',#23113,#4414);
#3664=LINE('',#23117,#4415);
#3665=LINE('',#23122,#4416);
#3666=LINE('',#23124,#4417);
#3667=LINE('',#23126,#4418);
#3668=LINE('',#23127,#4419);
#3669=LINE('',#23130,#4420);
#3670=LINE('',#23132,#4421);
#3671=LINE('',#23133,#4422);
#3672=LINE('',#23136,#4423);
#3673=LINE('',#23138,#4424);
#3674=LINE('',#23139,#4425);
#3675=LINE('',#23142,#4426);
#3676=LINE('',#23144,#4427);
#3677=LINE('',#23145,#4428);
#3678=LINE('',#23148,#4429);
#3679=LINE('',#23150,#4430);
#3680=LINE('',#23151,#4431);
#3681=LINE('',#23153,#4432);
#3682=LINE('',#23154,#4433);
#3683=LINE('',#23217,#4434);
#3684=LINE('',#23231,#4435);
#3685=LINE('',#23234,#4436);
#3686=LINE('',#23247,#4437);
#3687=LINE('',#23250,#4438);
#3688=LINE('',#23258,#4439);
#3689=LINE('',#23265,#4440);
#3690=LINE('',#23267,#4441);
#3691=LINE('',#23274,#4442);
#3692=LINE('',#23307,#4443);
#3693=LINE('',#23349,#4444);
#3694=LINE('',#23353,#4445);
#3695=LINE('',#23355,#4446);
#3696=LINE('',#23360,#4447);
#3697=LINE('',#23362,#4448);
#3698=LINE('',#23370,#4449);
#3699=LINE('',#23372,#4450);
#3700=LINE('',#23374,#4451);
#3701=LINE('',#23375,#4452);
#3702=LINE('',#23378,#4453);
#3703=LINE('',#23380,#4454);
#3704=LINE('',#23381,#4455);
#3705=LINE('',#23384,#4456);
#3706=LINE('',#23386,#4457);
#3707=LINE('',#23387,#4458);
#3708=LINE('',#23390,#4459);
#3709=LINE('',#23392,#4460);
#3710=LINE('',#23393,#4461);
#3711=LINE('',#23396,#4462);
#3712=LINE('',#23398,#4463);
#3713=LINE('',#23399,#4464);
#3714=LINE('',#23401,#4465);
#3715=LINE('',#23402,#4466);
#3716=LINE('',#23410,#4467);
#3717=LINE('',#23414,#4468);
#3718=LINE('',#23418,#4469);
#3719=VECTOR('',#14527,0.165);
#3720=VECTOR('',#14536,0.165);
#3721=VECTOR('',#14545,0.164999999999999);
#3722=VECTOR('',#14554,0.164999999999999);
#3723=VECTOR('',#14563,0.165);
#3724=VECTOR('',#14572,0.165);
#3725=VECTOR('',#14581,0.165);
#3726=VECTOR('',#14590,0.165);
#3727=VECTOR('',#14599,0.165);
#3728=VECTOR('',#14608,0.165);
#3729=VECTOR('',#14617,0.164999999999999);
#3730=VECTOR('',#14626,0.164999999999999);
#3731=VECTOR('',#14635,0.165);
#3732=VECTOR('',#14644,0.164999999999999);
#3733=VECTOR('',#14651,1.);
#3734=VECTOR('',#14652,1.);
#3735=VECTOR('',#14653,1.);
#3736=VECTOR('',#14654,1.);
#3737=VECTOR('',#14657,1.);
#3738=VECTOR('',#14658,1.);
#3739=VECTOR('',#14659,1.);
#3740=VECTOR('',#14662,1.);
#3741=VECTOR('',#14663,1.);
#3742=VECTOR('',#14664,1.);
#3743=VECTOR('',#14667,1.);
#3744=VECTOR('',#14668,1.);
#3745=VECTOR('',#14677,1.);
#3746=VECTOR('',#14678,1.);
#3747=VECTOR('',#14679,1.);
#3748=VECTOR('',#14680,1.);
#3749=VECTOR('',#14683,1.);
#3750=VECTOR('',#14684,1.);
#3751=VECTOR('',#14685,1.);
#3752=VECTOR('',#14688,1.);
#3753=VECTOR('',#14689,1.);
#3754=VECTOR('',#14690,1.);
#3755=VECTOR('',#14693,1.);
#3756=VECTOR('',#14694,1.);
#3757=VECTOR('',#14703,1.);
#3758=VECTOR('',#14704,1.);
#3759=VECTOR('',#14705,1.);
#3760=VECTOR('',#14706,1.);
#3761=VECTOR('',#14709,1.);
#3762=VECTOR('',#14710,1.);
#3763=VECTOR('',#14711,1.);
#3764=VECTOR('',#14714,1.);
#3765=VECTOR('',#14715,1.);
#3766=VECTOR('',#14716,1.);
#3767=VECTOR('',#14719,1.);
#3768=VECTOR('',#14720,1.);
#3769=VECTOR('',#14731,0.165);
#3770=VECTOR('',#14738,0.165);
#3771=VECTOR('',#14745,0.165);
#3772=VECTOR('',#14752,0.165);
#3773=VECTOR('',#14759,1.5);
#3774=VECTOR('',#14766,0.225);
#3775=VECTOR('',#14773,0.225);
#3776=VECTOR('',#14780,0.225);
#3777=VECTOR('',#14787,0.225);
#3778=VECTOR('',#14792,1.);
#3779=VECTOR('',#14793,1.);
#3780=VECTOR('',#14794,1.);
#3781=VECTOR('',#14795,1.);
#3782=VECTOR('',#14798,1.);
#3783=VECTOR('',#14799,1.);
#3784=VECTOR('',#14800,1.);
#3785=VECTOR('',#14801,1.);
#3786=VECTOR('',#14804,1.);
#3787=VECTOR('',#14805,1.);
#3788=VECTOR('',#14806,1.);
#3789=VECTOR('',#14809,1.);
#3790=VECTOR('',#14810,1.);
#3791=VECTOR('',#14811,1.);
#3792=VECTOR('',#14814,1.);
#3793=VECTOR('',#14815,1.);
#3794=VECTOR('',#14816,1.);
#3795=VECTOR('',#14817,1.);
#3796=VECTOR('',#14820,1.);
#3797=VECTOR('',#14821,1.);
#3798=VECTOR('',#14824,1.);
#3799=VECTOR('',#14825,1.);
#3800=VECTOR('',#14826,1.);
#3801=VECTOR('',#14829,1.);
#3802=VECTOR('',#14840,1.1);
#3803=VECTOR('',#14847,1.49);
#3804=VECTOR('',#14858,1.);
#3805=VECTOR('',#14861,1.);
#3806=VECTOR('',#14866,1.);
#3807=VECTOR('',#14869,1.);
#3808=VECTOR('',#14874,1.);
#3809=VECTOR('',#14877,1.);
#3810=VECTOR('',#14882,1.);
#3811=VECTOR('',#14885,1.);
#3812=VECTOR('',#14920,1.49);
#3813=VECTOR('',#14929,1.1);
#3814=VECTOR('',#14936,1.);
#3815=VECTOR('',#14939,1.);
#3816=VECTOR('',#14944,1.);
#3817=VECTOR('',#14947,1.);
#3818=VECTOR('',#14952,1.);
#3819=VECTOR('',#14955,1.);
#3820=VECTOR('',#14960,1.);
#3821=VECTOR('',#14963,1.);
#3822=VECTOR('',#14996,1.49);
#3823=VECTOR('',#15007,1.1);
#3824=VECTOR('',#15016,0.4);
#3825=VECTOR('',#15027,0.4);
#3826=VECTOR('',#15038,0.225);
#3827=VECTOR('',#15043,0.225);
#3828=VECTOR('',#15048,0.8);
#3829=VECTOR('',#15053,1.);
#3830=VECTOR('',#15054,1.);
#3831=VECTOR('',#15055,1.);
#3832=VECTOR('',#15056,1.);
#3833=VECTOR('',#15059,1.);
#3834=VECTOR('',#15060,1.);
#3835=VECTOR('',#15061,1.);
#3836=VECTOR('',#15064,1.);
#3837=VECTOR('',#15065,1.);
#3838=VECTOR('',#15066,1.);
#3839=VECTOR('',#15069,1.);
#3840=VECTOR('',#15070,1.);
#3841=VECTOR('',#15081,0.605);
#3842=VECTOR('',#15088,0.8);
#3843=VECTOR('',#15101,0.399999999999999);
#3844=VECTOR('',#15112,0.399999999999999);
#3845=VECTOR('',#15123,0.225000000000001);
#3846=VECTOR('',#15128,0.225000000000001);
#3847=VECTOR('',#15133,0.8);
#3848=VECTOR('',#15138,1.);
#3849=VECTOR('',#15139,1.);
#3850=VECTOR('',#15140,1.);
#3851=VECTOR('',#15141,1.);
#3852=VECTOR('',#15144,1.);
#3853=VECTOR('',#15145,1.);
#3854=VECTOR('',#15146,1.);
#3855=VECTOR('',#15149,1.);
#3856=VECTOR('',#15150,1.);
#3857=VECTOR('',#15151,1.);
#3858=VECTOR('',#15154,1.);
#3859=VECTOR('',#15155,1.);
#3860=VECTOR('',#15166,0.605);
#3861=VECTOR('',#15173,0.8);
#3862=VECTOR('',#15186,0.31);
#3863=VECTOR('',#15193,0.8);
#3864=VECTOR('',#15204,0.4);
#3865=VECTOR('',#15207,1.);
#3866=VECTOR('',#15212,0.4);
#3867=VECTOR('',#15215,1.);
#3868=VECTOR('',#15222,1.);
#3869=VECTOR('',#15233,1.);
#3870=VECTOR('',#15242,1.);
#3871=VECTOR('',#15243,1.);
#3872=VECTOR('',#15244,1.);
#3873=VECTOR('',#15247,1.);
#3874=VECTOR('',#15248,1.);
#3875=VECTOR('',#15249,1.);
#3876=VECTOR('',#15252,1.);
#3877=VECTOR('',#15253,1.);
#3878=VECTOR('',#15254,1.);
#3879=VECTOR('',#15259,0.225);
#3880=VECTOR('',#15264,0.225);
#3881=VECTOR('',#15267,1.);
#3882=VECTOR('',#15274,1.);
#3883=VECTOR('',#15275,1.);
#3884=VECTOR('',#15276,1.);
#3885=VECTOR('',#15277,1.);
#3886=VECTOR('',#15280,1.);
#3887=VECTOR('',#15283,1.);
#3888=VECTOR('',#15284,1.);
#3889=VECTOR('',#15287,1.);
#3890=VECTOR('',#15288,1.);
#3891=VECTOR('',#15291,1.);
#3892=VECTOR('',#15300,0.375);
#3893=VECTOR('',#15311,0.375);
#3894=VECTOR('',#15322,0.375);
#3895=VECTOR('',#15333,0.375);
#3896=VECTOR('',#15344,0.225);
#3897=VECTOR('',#15349,0.225);
#3898=VECTOR('',#15354,0.225);
#3899=VECTOR('',#15359,0.225000000000001);
#3900=VECTOR('',#15362,1.);
#3901=VECTOR('',#15363,1.);
#3902=VECTOR('',#15364,1.);
#3903=VECTOR('',#15365,1.);
#3904=VECTOR('',#15368,1.);
#3905=VECTOR('',#15369,1.);
#3906=VECTOR('',#15370,1.);
#3907=VECTOR('',#15373,1.);
#3908=VECTOR('',#15374,1.);
#3909=VECTOR('',#15375,1.);
#3910=VECTOR('',#15378,1.);
#3911=VECTOR('',#15379,1.);
#3912=VECTOR('',#15380,1.);
#3913=VECTOR('',#15383,1.);
#3914=VECTOR('',#15384,1.);
#3915=VECTOR('',#15385,1.);
#3916=VECTOR('',#15388,1.);
#3917=VECTOR('',#15389,1.);
#3918=VECTOR('',#15390,1.);
#3919=VECTOR('',#15393,1.);
#3920=VECTOR('',#15394,1.);
#3921=VECTOR('',#15395,1.);
#3922=VECTOR('',#15398,1.);
#3923=VECTOR('',#15399,1.);
#3924=VECTOR('',#15400,1.);
#3925=VECTOR('',#15403,1.);
#3926=VECTOR('',#15404,1.);
#3927=VECTOR('',#15405,1.);
#3928=VECTOR('',#15408,1.);
#3929=VECTOR('',#15409,1.);
#3930=VECTOR('',#15410,1.);
#3931=VECTOR('',#15413,1.);
#3932=VECTOR('',#15414,1.);
#3933=VECTOR('',#15415,1.);
#3934=VECTOR('',#15418,1.);
#3935=VECTOR('',#15419,1.);
#3936=VECTOR('',#15442,0.976185);
#3937=VECTOR('',#15449,0.5);
#3938=VECTOR('',#15454,0.53);
#3939=VECTOR('',#15463,0.976185);
#3940=VECTOR('',#15470,0.53);
#3941=VECTOR('',#15489,1.023815);
#3942=VECTOR('',#15500,1.47);
#3943=VECTOR('',#15505,1.5);
#3944=VECTOR('',#15510,1.47);
#3945=VECTOR('',#15515,1.023815);
#3946=VECTOR('',#15566,1.019052);
#3947=VECTOR('',#15643,0.980948);
#3948=VECTOR('',#15672,1.013815);
#3949=VECTOR('',#15679,0.991185);
#3950=VECTOR('',#15690,1.013815);
#3951=VECTOR('',#15697,0.991185);
#3952=VECTOR('',#15716,0.225);
#3953=VECTOR('',#15723,0.225);
#3954=VECTOR('',#15730,0.164999999999999);
#3955=VECTOR('',#15737,0.165);
#3956=VECTOR('',#15744,0.165);
#3957=VECTOR('',#15751,0.164999999999999);
#3958=VECTOR('',#15758,0.275);
#3959=VECTOR('',#15765,0.275);
#3960=VECTOR('',#15772,0.275);
#3961=VECTOR('',#15779,0.275);
#3962=VECTOR('',#15784,1.);
#3963=VECTOR('',#15785,1.);
#3964=VECTOR('',#15786,1.);
#3965=VECTOR('',#15787,1.);
#3966=VECTOR('',#15790,1.);
#3967=VECTOR('',#15791,1.);
#3968=VECTOR('',#15792,1.);
#3969=VECTOR('',#15795,1.);
#3970=VECTOR('',#15796,1.);
#3971=VECTOR('',#15797,1.);
#3972=VECTOR('',#15800,1.);
#3973=VECTOR('',#15801,1.);
#3974=VECTOR('',#15812,0.164999999999999);
#3975=VECTOR('',#15819,0.164999999999999);
#3976=VECTOR('',#15826,0.164999999999999);
#3977=VECTOR('',#15833,0.164999999999999);
#3978=VECTOR('',#15840,1.6);
#3979=VECTOR('',#15845,1.);
#3980=VECTOR('',#15850,1.);
#3981=VECTOR('',#15853,1.);
#3982=VECTOR('',#15856,1.);
#3983=VECTOR('',#15861,1.);
#3984=VECTOR('',#15864,1.);
#3985=VECTOR('',#15867,1.);
#3986=VECTOR('',#15872,1.);
#3987=VECTOR('',#15875,1.);
#3988=VECTOR('',#15878,1.);
#3989=VECTOR('',#15883,1.);
#3990=VECTOR('',#15886,1.);
#3991=VECTOR('',#15889,1.);
#3992=VECTOR('',#15890,1.);
#3993=VECTOR('',#15891,1.);
#3994=VECTOR('',#15892,1.);
#3995=VECTOR('',#15893,1.);
#3996=VECTOR('',#15894,1.);
#3997=VECTOR('',#15895,1.);
#3998=VECTOR('',#15896,1.);
#3999=VECTOR('',#15897,1.);
#4000=VECTOR('',#15898,1.);
#4001=VECTOR('',#15901,1.);
#4002=VECTOR('',#15902,1.);
#4003=VECTOR('',#15903,1.);
#4004=VECTOR('',#15904,1.);
#4005=VECTOR('',#15905,1.);
#4006=VECTOR('',#15906,1.);
#4007=VECTOR('',#15907,1.);
#4008=VECTOR('',#15908,1.);
#4009=VECTOR('',#15909,1.);
#4010=VECTOR('',#15910,1.);
#4011=VECTOR('',#15915,0.225);
#4012=VECTOR('',#15922,0.225);
#4013=VECTOR('',#15929,0.225);
#4014=VECTOR('',#15936,0.225);
#4015=VECTOR('',#15941,1.);
#4016=VECTOR('',#15942,1.);
#4017=VECTOR('',#15945,1.);
#4018=VECTOR('',#15946,1.);
#4019=VECTOR('',#15949,1.);
#4020=VECTOR('',#15952,1.);
#4021=VECTOR('',#15955,1.);
#4022=VECTOR('',#15958,1.);
#4023=VECTOR('',#15969,1.2);
#4024=VECTOR('',#15976,1.59);
#4025=VECTOR('',#15987,1.);
#4026=VECTOR('',#15990,1.);
#4027=VECTOR('',#15995,1.);
#4028=VECTOR('',#15998,1.);
#4029=VECTOR('',#16003,1.);
#4030=VECTOR('',#16006,1.);
#4031=VECTOR('',#16011,1.);
#4032=VECTOR('',#16014,1.);
#4033=VECTOR('',#16049,1.59);
#4034=VECTOR('',#16058,1.2);
#4035=VECTOR('',#16065,1.);
#4036=VECTOR('',#16068,1.);
#4037=VECTOR('',#16073,1.);
#4038=VECTOR('',#16076,1.);
#4039=VECTOR('',#16081,1.);
#4040=VECTOR('',#16084,1.);
#4041=VECTOR('',#16089,1.);
#4042=VECTOR('',#16092,1.);
#4043=VECTOR('',#16125,1.59);
#4044=VECTOR('',#16136,1.2);
#4045=VECTOR('',#16145,0.164999999999999);
#4046=VECTOR('',#16154,0.164999999999999);
#4047=VECTOR('',#16163,0.34);
#4048=VECTOR('',#16168,1.);
#4049=VECTOR('',#16169,1.);
#4050=VECTOR('',#16170,1.);
#4051=VECTOR('',#16171,1.);
#4052=VECTOR('',#16174,1.);
#4053=VECTOR('',#16175,1.);
#4054=VECTOR('',#16176,1.);
#4055=VECTOR('',#16179,1.);
#4056=VECTOR('',#16180,1.);
#4057=VECTOR('',#16181,1.);
#4058=VECTOR('',#16184,1.);
#4059=VECTOR('',#16185,1.);
#4060=VECTOR('',#16198,0.3);
#4061=VECTOR('',#16207,1.);
#4062=VECTOR('',#16214,0.164999999999999);
#4063=VECTOR('',#16219,1.);
#4064=VECTOR('',#16224,0.3);
#4065=VECTOR('',#16225,0.3);
#4066=VECTOR('',#16230,1.);
#4067=VECTOR('',#16231,1.);
#4068=VECTOR('',#16232,1.);
#4069=VECTOR('',#16233,1.);
#4070=VECTOR('',#16236,1.);
#4071=VECTOR('',#16237,1.);
#4072=VECTOR('',#16238,1.);
#4073=VECTOR('',#16241,1.);
#4074=VECTOR('',#16242,1.);
#4075=VECTOR('',#16243,1.);
#4076=VECTOR('',#16246,1.);
#4077=VECTOR('',#16247,1.);
#4078=VECTOR('',#16258,1.);
#4079=VECTOR('',#16263,1.);
#4080=VECTOR('',#16266,0.21);
#4081=VECTOR('',#16271,1.);
#4082=VECTOR('',#16274,1.);
#4083=VECTOR('',#16279,1.);
#4084=VECTOR('',#16282,0.21);
#4085=VECTOR('',#16287,1.);
#4086=VECTOR('',#16290,1.);
#4087=VECTOR('',#16295,1.);
#4088=VECTOR('',#16298,0.21);
#4089=VECTOR('',#16303,1.);
#4090=VECTOR('',#16306,1.);
#4091=VECTOR('',#16311,1.);
#4092=VECTOR('',#16314,0.21);
#4093=VECTOR('',#16319,1.);
#4094=VECTOR('',#16322,1.);
#4095=VECTOR('',#16323,1.);
#4096=VECTOR('',#16324,1.);
#4097=VECTOR('',#16325,1.);
#4098=VECTOR('',#16326,1.);
#4099=VECTOR('',#16327,1.);
#4100=VECTOR('',#16330,1.);
#4101=VECTOR('',#16331,1.);
#4102=VECTOR('',#16332,1.);
#4103=VECTOR('',#16333,1.);
#4104=VECTOR('',#16334,1.);
#4105=VECTOR('',#16335,1.);
#4106=VECTOR('',#16338,1.);
#4107=VECTOR('',#16339,1.);
#4108=VECTOR('',#16340,1.);
#4109=VECTOR('',#16341,1.);
#4110=VECTOR('',#16342,1.);
#4111=VECTOR('',#16343,1.);
#4112=VECTOR('',#16344,1.);
#4113=VECTOR('',#16345,1.);
#4114=VECTOR('',#16346,1.);
#4115=VECTOR('',#16347,1.);
#4116=VECTOR('',#16350,1.);
#4117=VECTOR('',#16351,1.);
#4118=VECTOR('',#16354,1.);
#4119=VECTOR('',#16355,1.);
#4120=VECTOR('',#16358,1.);
#4121=VECTOR('',#16359,1.);
#4122=VECTOR('',#16362,1.);
#4123=VECTOR('',#16363,1.);
#4124=VECTOR('',#16366,1.);
#4125=VECTOR('',#16369,1.);
#4126=VECTOR('',#16370,1.);
#4127=VECTOR('',#16373,1.);
#4128=VECTOR('',#16374,1.);
#4129=VECTOR('',#16377,1.);
#4130=VECTOR('',#16378,1.);
#4131=VECTOR('',#16381,1.);
#4132=VECTOR('',#16382,1.);
#4133=VECTOR('',#16385,1.);
#4134=VECTOR('',#16392,1.);
#4135=VECTOR('',#16393,1.);
#4136=VECTOR('',#16394,1.);
#4137=VECTOR('',#16395,1.);
#4138=VECTOR('',#16398,1.);
#4139=VECTOR('',#16399,1.);
#4140=VECTOR('',#16400,1.);
#4141=VECTOR('',#16403,1.);
#4142=VECTOR('',#16404,1.);
#4143=VECTOR('',#16405,1.);
#4144=VECTOR('',#16408,1.);
#4145=VECTOR('',#16409,1.);
#4146=VECTOR('',#16410,1.);
#4147=VECTOR('',#16413,1.);
#4148=VECTOR('',#16414,1.);
#4149=VECTOR('',#16415,1.);
#4150=VECTOR('',#16418,1.);
#4151=VECTOR('',#16419,1.);
#4152=VECTOR('',#16420,1.);
#4153=VECTOR('',#16423,1.);
#4154=VECTOR('',#16424,1.);
#4155=VECTOR('',#16425,1.);
#4156=VECTOR('',#16428,1.);
#4157=VECTOR('',#16429,1.);
#4158=VECTOR('',#16438,1.);
#4159=VECTOR('',#16439,1.);
#4160=VECTOR('',#16440,1.);
#4161=VECTOR('',#16441,1.);
#4162=VECTOR('',#16444,1.);
#4163=VECTOR('',#16445,1.);
#4164=VECTOR('',#16446,1.);
#4165=VECTOR('',#16449,1.);
#4166=VECTOR('',#16450,1.);
#4167=VECTOR('',#16451,1.);
#4168=VECTOR('',#16454,1.);
#4169=VECTOR('',#16455,1.);
#4170=VECTOR('',#16456,1.);
#4171=VECTOR('',#16459,1.);
#4172=VECTOR('',#16460,1.);
#4173=VECTOR('',#16461,1.);
#4174=VECTOR('',#16464,1.);
#4175=VECTOR('',#16465,1.);
#4176=VECTOR('',#16466,1.);
#4177=VECTOR('',#16469,1.);
#4178=VECTOR('',#16470,1.);
#4179=VECTOR('',#16471,1.);
#4180=VECTOR('',#16474,1.);
#4181=VECTOR('',#16475,1.);
#4182=VECTOR('',#16490,1.);
#4183=VECTOR('',#16491,1.);
#4184=VECTOR('',#16492,1.);
#4185=VECTOR('',#16493,1.);
#4186=VECTOR('',#16496,1.);
#4187=VECTOR('',#16497,1.);
#4188=VECTOR('',#16498,1.);
#4189=VECTOR('',#16501,1.);
#4190=VECTOR('',#16502,1.);
#4191=VECTOR('',#16503,1.);
#4192=VECTOR('',#16506,1.);
#4193=VECTOR('',#16507,1.);
#4194=VECTOR('',#16508,1.);
#4195=VECTOR('',#16511,1.);
#4196=VECTOR('',#16512,1.);
#4197=VECTOR('',#16513,1.);
#4198=VECTOR('',#16516,1.);
#4199=VECTOR('',#16517,1.);
#4200=VECTOR('',#16534,0.4);
#4201=VECTOR('',#16539,0.425);
#4202=VECTOR('',#16544,0.41);
#4203=VECTOR('',#16553,0.26);
#4204=VECTOR('',#16556,0.25);
#4205=VECTOR('',#16575,1.070235);
#4206=VECTOR('',#16582,0.6);
#4207=VECTOR('',#16587,0.63);
#4208=VECTOR('',#16596,1.070235);
#4209=VECTOR('',#16603,0.63);
#4210=VECTOR('',#16622,1.129765);
#4211=VECTOR('',#16633,1.57);
#4212=VECTOR('',#16638,1.6);
#4213=VECTOR('',#16643,1.57);
#4214=VECTOR('',#16648,1.129765);
#4215=VECTOR('',#16695,1.123812);
#4216=VECTOR('',#16764,1.076188);
#4217=VECTOR('',#16793,1.119765);
#4218=VECTOR('',#16800,1.085235);
#4219=VECTOR('',#16811,1.119765);
#4220=VECTOR('',#16818,1.085235);
#4221=VECTOR('',#16833,1.);
#4222=VECTOR('',#16834,1.);
#4223=VECTOR('',#16835,1.);
#4224=VECTOR('',#16836,1.);
#4225=VECTOR('',#16839,1.);
#4226=VECTOR('',#16840,1.);
#4227=VECTOR('',#16841,1.);
#4228=VECTOR('',#16844,1.);
#4229=VECTOR('',#16845,1.);
#4230=VECTOR('',#16846,1.);
#4231=VECTOR('',#16849,1.);
#4232=VECTOR('',#16850,1.);
#4233=VECTOR('',#16851,1.);
#4234=VECTOR('',#16854,1.);
#4235=VECTOR('',#16855,1.);
#4236=VECTOR('',#16856,1.);
#4237=VECTOR('',#16859,1.);
#4238=VECTOR('',#16860,1.);
#4239=VECTOR('',#16877,0.325);
#4240=VECTOR('',#16882,0.35);
#4241=VECTOR('',#16887,0.335);
#4242=VECTOR('',#16896,0.21);
#4243=VECTOR('',#16899,0.2);
#4244=VECTOR('',#16908,0.165);
#4245=VECTOR('',#16927,0.7);
#4246=VECTOR('',#16930,0.5);
#4247=VECTOR('',#16937,0.4);
#4248=VECTOR('',#16946,0.5);
#4249=VECTOR('',#16957,0.505);
#4250=VECTOR('',#16966,0.405);
#4251=VECTOR('',#16973,0.7);
#4252=VECTOR('',#16986,0.505);
#4253=VECTOR('',#16993,0.7);
#4254=VECTOR('',#17006,0.15);
#4255=VECTOR('',#17019,0.15);
#4256=VECTOR('',#17032,0.225);
#4257=VECTOR('',#17039,0.6);
#4258=VECTOR('',#17050,0.125);
#4259=VECTOR('',#17053,0.125);
#4260=VECTOR('',#17058,0.65);
#4261=VECTOR('',#17059,0.65);
#4262=VECTOR('',#17064,0.125);
#4263=VECTOR('',#17067,0.125);
#4264=VECTOR('',#17072,0.4);
#4265=VECTOR('',#17073,0.4);
#4266=VECTOR('',#17166,0.8);
#4267=VECTOR('',#17257,0.8);
#4268=VECTOR('',#17262,1.);
#4269=VECTOR('',#17263,1.);
#4270=VECTOR('',#17266,1.);
#4271=VECTOR('',#17269,1.);
#4272=VECTOR('',#17272,1.);
#4273=VECTOR('',#17275,1.);
#4274=VECTOR('',#17278,1.);
#4275=VECTOR('',#17281,1.);
#4276=VECTOR('',#17284,1.);
#4277=VECTOR('',#17287,1.);
#4278=VECTOR('',#17290,1.);
#4279=VECTOR('',#17293,1.);
#4280=VECTOR('',#17296,1.);
#4281=VECTOR('',#17299,1.);
#4282=VECTOR('',#17302,1.);
#4283=VECTOR('',#17305,1.);
#4284=VECTOR('',#17308,1.);
#4285=VECTOR('',#17311,1.);
#4286=VECTOR('',#17314,1.);
#4287=VECTOR('',#17317,1.);
#4288=VECTOR('',#17320,1.);
#4289=VECTOR('',#17323,1.);
#4290=VECTOR('',#17326,1.);
#4291=VECTOR('',#17329,1.);
#4292=VECTOR('',#17332,1.);
#4293=VECTOR('',#17335,1.);
#4294=VECTOR('',#17338,1.);
#4295=VECTOR('',#17341,1.);
#4296=VECTOR('',#17344,1.);
#4297=VECTOR('',#17347,1.);
#4298=VECTOR('',#17350,1.);
#4299=VECTOR('',#17353,1.);
#4300=VECTOR('',#17356,1.);
#4301=VECTOR('',#17359,1.);
#4302=VECTOR('',#17362,1.);
#4303=VECTOR('',#17365,1.);
#4304=VECTOR('',#17368,1.);
#4305=VECTOR('',#17371,1.);
#4306=VECTOR('',#17374,1.);
#4307=VECTOR('',#17377,1.);
#4308=VECTOR('',#17388,0.164999999999999);
#4309=VECTOR('',#17407,0.800000000000001);
#4310=VECTOR('',#17410,0.6);
#4311=VECTOR('',#17419,0.6);
#4312=VECTOR('',#17428,0.605);
#4313=VECTOR('',#17435,0.800000000000001);
#4314=VECTOR('',#17448,0.605);
#4315=VECTOR('',#17455,0.800000000000001);
#4316=VECTOR('',#17468,0.15);
#4317=VECTOR('',#17481,0.15);
#4318=VECTOR('',#17494,0.225);
#4319=VECTOR('',#17501,0.800000000000001);
#4320=VECTOR('',#17512,0.125);
#4321=VECTOR('',#17515,0.125);
#4322=VECTOR('',#17520,1.);
#4323=VECTOR('',#17521,1.);
#4324=VECTOR('',#17526,0.125);
#4325=VECTOR('',#17529,0.125);
#4326=VECTOR('',#17534,0.6);
#4327=VECTOR('',#17535,0.6);
#4328=VECTOR('',#17708,1.4);
#4329=VECTOR('',#17879,1.4);
#4330=VECTOR('',#17884,1.);
#4331=VECTOR('',#17885,1.);
#4332=VECTOR('',#17888,1.);
#4333=VECTOR('',#17891,1.);
#4334=VECTOR('',#17894,1.);
#4335=VECTOR('',#17897,1.);
#4336=VECTOR('',#17900,1.);
#4337=VECTOR('',#17903,1.);
#4338=VECTOR('',#17906,1.);
#4339=VECTOR('',#17909,1.);
#4340=VECTOR('',#17912,1.);
#4341=VECTOR('',#17915,1.);
#4342=VECTOR('',#17918,1.);
#4343=VECTOR('',#17921,1.);
#4344=VECTOR('',#17924,1.);
#4345=VECTOR('',#17927,1.);
#4346=VECTOR('',#17930,1.);
#4347=VECTOR('',#17933,1.);
#4348=VECTOR('',#17936,1.);
#4349=VECTOR('',#17939,1.);
#4350=VECTOR('',#17942,1.);
#4351=VECTOR('',#17945,1.);
#4352=VECTOR('',#17948,1.);
#4353=VECTOR('',#17951,1.);
#4354=VECTOR('',#17954,1.);
#4355=VECTOR('',#17957,1.);
#4356=VECTOR('',#17960,1.);
#4357=VECTOR('',#17963,1.);
#4358=VECTOR('',#17966,1.);
#4359=VECTOR('',#17969,1.);
#4360=VECTOR('',#17972,1.);
#4361=VECTOR('',#17975,1.);
#4362=VECTOR('',#17978,1.);
#4363=VECTOR('',#17981,1.);
#4364=VECTOR('',#17984,1.);
#4365=VECTOR('',#17987,1.);
#4366=VECTOR('',#17990,1.);
#4367=VECTOR('',#17993,1.);
#4368=VECTOR('',#17996,1.);
#4369=VECTOR('',#17999,1.);
#4370=VECTOR('',#18002,1.);
#4371=VECTOR('',#18005,1.);
#4372=VECTOR('',#18008,1.);
#4373=VECTOR('',#18011,1.);
#4374=VECTOR('',#18014,1.);
#4375=VECTOR('',#18017,1.);
#4376=VECTOR('',#18020,1.);
#4377=VECTOR('',#18023,1.);
#4378=VECTOR('',#18026,1.);
#4379=VECTOR('',#18029,1.);
#4380=VECTOR('',#18032,1.);
#4381=VECTOR('',#18035,1.);
#4382=VECTOR('',#18038,1.);
#4383=VECTOR('',#18041,1.);
#4384=VECTOR('',#18044,1.);
#4385=VECTOR('',#18047,1.);
#4386=VECTOR('',#18050,1.);
#4387=VECTOR('',#18053,1.);
#4388=VECTOR('',#18056,1.);
#4389=VECTOR('',#18059,1.);
#4390=VECTOR('',#18062,1.);
#4391=VECTOR('',#18065,1.);
#4392=VECTOR('',#18068,1.);
#4393=VECTOR('',#18071,1.);
#4394=VECTOR('',#18074,1.);
#4395=VECTOR('',#18077,1.);
#4396=VECTOR('',#18080,1.);
#4397=VECTOR('',#18083,1.);
#4398=VECTOR('',#18086,1.);
#4399=VECTOR('',#18089,1.);
#4400=VECTOR('',#18092,1.);
#4401=VECTOR('',#18095,1.);
#4402=VECTOR('',#18098,1.);
#4403=VECTOR('',#18101,1.);
#4404=VECTOR('',#18104,1.);
#4405=VECTOR('',#18107,1.);
#4406=VECTOR('',#18110,1.);
#4407=VECTOR('',#18113,1.);
#4408=VECTOR('',#18116,1.);
#4409=VECTOR('',#18119,1.);
#4410=VECTOR('',#18132,0.325);
#4411=VECTOR('',#18137,0.35);
#4412=VECTOR('',#18142,0.335);
#4413=VECTOR('',#18151,0.21);
#4414=VECTOR('',#18156,0.2);
#4415=VECTOR('',#18161,0.18);
#4416=VECTOR('',#18166,1.);
#4417=VECTOR('',#18167,1.);
#4418=VECTOR('',#18168,1.);
#4419=VECTOR('',#18169,1.);
#4420=VECTOR('',#18172,1.);
#4421=VECTOR('',#18173,1.);
#4422=VECTOR('',#18174,1.);
#4423=VECTOR('',#18177,1.);
#4424=VECTOR('',#18178,1.);
#4425=VECTOR('',#18179,1.);
#4426=VECTOR('',#18182,1.);
#4427=VECTOR('',#18183,1.);
#4428=VECTOR('',#18184,1.);
#4429=VECTOR('',#18187,1.);
#4430=VECTOR('',#18188,1.);
#4431=VECTOR('',#18189,1.);
#4432=VECTOR('',#18192,1.);
#4433=VECTOR('',#18193,1.);
#4434=VECTOR('',#18314,0.4);
#4435=VECTOR('',#18333,0.9);
#4436=VECTOR('',#18336,0.6);
#4437=VECTOR('',#18353,0.9);
#4438=VECTOR('',#18356,0.6);
#4439=VECTOR('',#18367,0.6);
#4440=VECTOR('',#18376,0.6);
#4441=VECTOR('',#18379,0.4);
#4442=VECTOR('',#18388,1.);
#4443=VECTOR('',#18395,0.165);
#4444=VECTOR('',#18398,1.);
#4445=VECTOR('',#18403,0.4);
#4446=VECTOR('',#18404,0.4);
#4447=VECTOR('',#18411,1.5);
#4448=VECTOR('',#18412,1.5);
#4449=VECTOR('',#18423,1.);
#4450=VECTOR('',#18424,1.);
#4451=VECTOR('',#18425,1.);
#4452=VECTOR('',#18426,1.);
#4453=VECTOR('',#18429,1.);
#4454=VECTOR('',#18430,1.);
#4455=VECTOR('',#18431,1.);
#4456=VECTOR('',#18434,1.);
#4457=VECTOR('',#18435,1.);
#4458=VECTOR('',#18436,1.);
#4459=VECTOR('',#18439,1.);
#4460=VECTOR('',#18440,1.);
#4461=VECTOR('',#18441,1.);
#4462=VECTOR('',#18444,1.);
#4463=VECTOR('',#18445,1.);
#4464=VECTOR('',#18446,1.);
#4465=VECTOR('',#18449,1.);
#4466=VECTOR('',#18450,1.);
#4467=VECTOR('',#18461,0.185);
#4468=VECTOR('',#18466,0.2);
#4469=VECTOR('',#18471,0.1625);
#4470=CIRCLE('',#12880,0.165);
#4471=CIRCLE('',#12881,0.165);
#4472=CIRCLE('',#12884,0.165);
#4473=CIRCLE('',#12885,0.165);
#4474=CIRCLE('',#12888,0.164999999999999);
#4475=CIRCLE('',#12889,0.164999999999999);
#4476=CIRCLE('',#12892,0.164999999999999);
#4477=CIRCLE('',#12893,0.164999999999999);
#4478=CIRCLE('',#12896,0.165);
#4479=CIRCLE('',#12897,0.165);
#4480=CIRCLE('',#12900,0.165);
#4481=CIRCLE('',#12901,0.165);
#4482=CIRCLE('',#12904,0.165);
#4483=CIRCLE('',#12905,0.165);
#4484=CIRCLE('',#12908,0.165);
#4485=CIRCLE('',#12909,0.165);
#4486=CIRCLE('',#12912,0.165);
#4487=CIRCLE('',#12913,0.165);
#4488=CIRCLE('',#12916,0.165);
#4489=CIRCLE('',#12917,0.165);
#4490=CIRCLE('',#12920,0.164999999999999);
#4491=CIRCLE('',#12921,0.164999999999999);
#4492=CIRCLE('',#12924,0.164999999999999);
#4493=CIRCLE('',#12925,0.164999999999999);
#4494=CIRCLE('',#12928,0.165);
#4495=CIRCLE('',#12929,0.165);
#4496=CIRCLE('',#12932,0.164999999999999);
#4497=CIRCLE('',#12933,0.164999999999999);
#4498=CIRCLE('',#12957,0.165);
#4499=CIRCLE('',#12958,0.165);
#4500=CIRCLE('',#12960,0.165);
#4501=CIRCLE('',#12961,0.165);
#4502=CIRCLE('',#12963,0.165);
#4503=CIRCLE('',#12964,0.165);
#4504=CIRCLE('',#12966,0.165);
#4505=CIRCLE('',#12967,0.165);
#4506=CIRCLE('',#12969,1.5);
#4507=CIRCLE('',#12970,1.5);
#4508=CIRCLE('',#12972,0.225);
#4509=CIRCLE('',#12973,0.225);
#4510=CIRCLE('',#12975,0.225);
#4511=CIRCLE('',#12976,0.225);
#4512=CIRCLE('',#12978,0.225);
#4513=CIRCLE('',#12979,0.225);
#4514=CIRCLE('',#12981,0.225);
#4515=CIRCLE('',#12982,0.225);
#4516=CIRCLE('',#12995,1.1);
#4517=CIRCLE('',#12996,1.1);
#4518=CIRCLE('',#12998,1.49);
#4519=CIRCLE('',#12999,1.49);
#4520=CIRCLE('',#13004,0.225);
#4521=CIRCLE('',#13005,0.225);
#4522=CIRCLE('',#13007,0.225);
#4523=CIRCLE('',#13008,0.225);
#4524=CIRCLE('',#13010,0.225);
#4525=CIRCLE('',#13011,0.225);
#4526=CIRCLE('',#13013,0.225);
#4527=CIRCLE('',#13014,0.225);
#4528=CIRCLE('',#13016,2.1);
#4529=CIRCLE('',#13017,2.1);
#4530=CIRCLE('',#13018,2.1);
#4531=CIRCLE('',#13019,2.1);
#4532=CIRCLE('',#13020,1.1);
#4533=CIRCLE('',#13022,2.1);
#4534=CIRCLE('',#13024,2.1);
#4535=CIRCLE('',#13026,2.1);
#4536=CIRCLE('',#13028,2.1);
#4537=CIRCLE('',#13030,1.49);
#4538=CIRCLE('',#13031,1.49);
#4539=CIRCLE('',#13033,1.1);
#4540=CIRCLE('',#13038,0.225);
#4541=CIRCLE('',#13039,0.225);
#4542=CIRCLE('',#13041,0.225);
#4543=CIRCLE('',#13042,0.225);
#4544=CIRCLE('',#13044,0.225);
#4545=CIRCLE('',#13045,0.225);
#4546=CIRCLE('',#13047,0.225);
#4547=CIRCLE('',#13048,0.225);
#4548=CIRCLE('',#13050,2.1);
#4549=CIRCLE('',#13051,2.1);
#4550=CIRCLE('',#13052,2.1);
#4551=CIRCLE('',#13053,2.1);
#4552=CIRCLE('',#13054,1.49);
#4553=CIRCLE('',#13056,2.1);
#4554=CIRCLE('',#13058,2.1);
#4555=CIRCLE('',#13060,2.1);
#4556=CIRCLE('',#13062,2.1);
#4557=CIRCLE('',#13064,1.49);
#4558=CIRCLE('',#13066,1.1);
#4559=CIRCLE('',#13068,1.1);
#4560=CIRCLE('',#13072,0.4);
#4561=CIRCLE('',#13073,0.4);
#4562=CIRCLE('',#13075,0.225);
#4563=CIRCLE('',#13077,0.4);
#4564=CIRCLE('',#13078,0.4);
#4565=CIRCLE('',#13080,0.225);
#4566=CIRCLE('',#13082,0.225);
#4567=CIRCLE('',#13084,0.225);
#4568=CIRCLE('',#13086,0.8);
#4569=CIRCLE('',#13087,0.8);
#4570=CIRCLE('',#13096,0.605);
#4571=CIRCLE('',#13097,0.605);
#4572=CIRCLE('',#13099,0.8);
#4573=CIRCLE('',#13100,0.8);
#4574=CIRCLE('',#13105,0.399999999999999);
#4575=CIRCLE('',#13106,0.399999999999999);
#4576=CIRCLE('',#13108,0.225000000000001);
#4577=CIRCLE('',#13110,0.399999999999999);
#4578=CIRCLE('',#13111,0.399999999999999);
#4579=CIRCLE('',#13113,0.225000000000001);
#4580=CIRCLE('',#13115,0.225000000000001);
#4581=CIRCLE('',#13117,0.225000000000001);
#4582=CIRCLE('',#13119,0.8);
#4583=CIRCLE('',#13120,0.8);
#4584=CIRCLE('',#13129,0.605);
#4585=CIRCLE('',#13130,0.605);
#4586=CIRCLE('',#13132,0.8);
#4587=CIRCLE('',#13133,0.8);
#4588=CIRCLE('',#13138,0.31);
#4589=CIRCLE('',#13139,0.31);
#4590=CIRCLE('',#13141,0.8);
#4591=CIRCLE('',#13142,0.8);
#4592=CIRCLE('',#13147,0.4);
#4593=CIRCLE('',#13148,0.4);
#4594=CIRCLE('',#13150,0.4);
#4595=CIRCLE('',#13151,0.4);
#4596=CIRCLE('',#13153,0.4);
#4597=CIRCLE('',#13154,0.4);
#4598=CIRCLE('',#13156,0.225);
#4599=CIRCLE('',#13158,0.4);
#4600=CIRCLE('',#13159,0.4);
#4601=CIRCLE('',#13161,0.225);
#4602=CIRCLE('',#13166,0.225);
#4603=CIRCLE('',#13168,0.225);
#4604=CIRCLE('',#13170,0.8);
#4605=CIRCLE('',#13171,0.8);
#4606=CIRCLE('',#13180,0.375);
#4607=CIRCLE('',#13181,0.375);
#4608=CIRCLE('',#13183,0.225);
#4609=CIRCLE('',#13185,0.375);
#4610=CIRCLE('',#13186,0.375);
#4611=CIRCLE('',#13188,0.225);
#4612=CIRCLE('',#13190,0.375);
#4613=CIRCLE('',#13191,0.375);
#4614=CIRCLE('',#13193,0.225);
#4615=CIRCLE('',#13195,0.375);
#4616=CIRCLE('',#13196,0.375);
#4617=CIRCLE('',#13198,0.225000000000001);
#4618=CIRCLE('',#13200,0.225);
#4619=CIRCLE('',#13202,0.225);
#4620=CIRCLE('',#13204,0.225);
#4621=CIRCLE('',#13206,0.225000000000001);
#4622=CIRCLE('',#13224,0.976185);
#4623=CIRCLE('',#13225,0.976185);
#4624=CIRCLE('',#13226,0.247676);
#4625=CIRCLE('',#13227,0.976185);
#4626=CIRCLE('',#13228,0.976185);
#4627=CIRCLE('',#13230,0.976185);
#4628=CIRCLE('',#13232,0.5);
#4629=CIRCLE('',#13233,0.5);
#4630=CIRCLE('',#13235,0.56);
#4631=CIRCLE('',#13238,0.976185);
#4632=CIRCLE('',#13240,0.56);
#4633=CIRCLE('',#13244,1.023815);
#4634=CIRCLE('',#13245,1.023815);
#4635=CIRCLE('',#13246,0.247676);
#4636=CIRCLE('',#13247,1.023815);
#4637=CIRCLE('',#13248,1.023815);
#4638=CIRCLE('',#13250,1.023815);
#4639=CIRCLE('',#13252,1.44);
#4640=CIRCLE('',#13253,1.023815);
#4641=CIRCLE('',#13255,1.5);
#4642=CIRCLE('',#13257,1.5);
#4643=CIRCLE('',#13259,1.44);
#4644=CIRCLE('',#13264,0.23815);
#4645=CIRCLE('',#13266,0.23815);
#4646=CIRCLE('',#13268,0.23815);
#4647=CIRCLE('',#13270,0.23815);
#4648=CIRCLE('',#13272,0.23815);
#4649=CIRCLE('',#13274,0.23815);
#4650=CIRCLE('',#13276,0.23815);
#4651=CIRCLE('',#13278,0.23815);
#4652=CIRCLE('',#13281,0.243053047864041);
#4653=CIRCLE('',#13282,0.243053047864041);
#4654=CIRCLE('',#13284,1.019052);
#4655=CIRCLE('',#13285,1.019052);
#4656=CIRCLE('',#13286,1.019052);
#4657=CIRCLE('',#13287,1.019052);
#4658=CIRCLE('',#13288,1.019052);
#4659=CIRCLE('',#13289,1.019052);
#4660=CIRCLE('',#13290,1.019052);
#4661=CIRCLE('',#13291,1.019052);
#4662=CIRCLE('',#13292,1.019052);
#4663=CIRCLE('',#13294,0.980948);
#4664=CIRCLE('',#13295,0.243053047864041);
#4665=CIRCLE('',#13297,0.243053047864041);
#4666=CIRCLE('',#13299,0.980948);
#4667=CIRCLE('',#13300,0.243053047864041);
#4668=CIRCLE('',#13302,0.243053047864041);
#4669=CIRCLE('',#13304,0.980948);
#4670=CIRCLE('',#13305,0.243053047864041);
#4671=CIRCLE('',#13307,0.243053047864041);
#4672=CIRCLE('',#13309,0.980948);
#4673=CIRCLE('',#13310,0.243053047864041);
#4674=CIRCLE('',#13312,0.243053047864041);
#4675=CIRCLE('',#13314,0.980948);
#4676=CIRCLE('',#13315,0.243053047864041);
#4677=CIRCLE('',#13317,0.243053047864041);
#4678=CIRCLE('',#13319,0.980948);
#4679=CIRCLE('',#13320,0.243053047864041);
#4680=CIRCLE('',#13322,0.243053047864041);
#4681=CIRCLE('',#13324,0.980948);
#4682=CIRCLE('',#13325,0.980948);
#4683=CIRCLE('',#13326,0.980948);
#4684=CIRCLE('',#13328,0.243053047864041);
#4685=CIRCLE('',#13330,0.243053047864041);
#4686=CIRCLE('',#13335,1.013815);
#4687=CIRCLE('',#13336,0.991185);
#4688=CIRCLE('',#13338,1.013815);
#4689=CIRCLE('',#13340,0.991185);
#4690=CIRCLE('',#13343,1.013815);
#4691=CIRCLE('',#13344,0.991185);
#4692=CIRCLE('',#13346,1.013815);
#4693=CIRCLE('',#13348,0.991185);
#4694=CIRCLE('',#13358,0.225);
#4695=CIRCLE('',#13359,0.225);
#4696=CIRCLE('',#13361,0.225);
#4697=CIRCLE('',#13362,0.225);
#4698=CIRCLE('',#13364,0.164999999999999);
#4699=CIRCLE('',#13365,0.164999999999999);
#4700=CIRCLE('',#13367,0.165);
#4701=CIRCLE('',#13368,0.165);
#4702=CIRCLE('',#13370,0.165);
#4703=CIRCLE('',#13371,0.165);
#4704=CIRCLE('',#13373,0.164999999999999);
#4705=CIRCLE('',#13374,0.164999999999999);
#4706=CIRCLE('',#13376,0.275);
#4707=CIRCLE('',#13377,0.275);
#4708=CIRCLE('',#13379,0.275);
#4709=CIRCLE('',#13380,0.275);
#4710=CIRCLE('',#13382,0.275);
#4711=CIRCLE('',#13383,0.275);
#4712=CIRCLE('',#13385,0.275);
#4713=CIRCLE('',#13386,0.275);
#4714=CIRCLE('',#13395,0.164999999999999);
#4715=CIRCLE('',#13396,0.164999999999999);
#4716=CIRCLE('',#13398,0.164999999999999);
#4717=CIRCLE('',#13399,0.164999999999999);
#4718=CIRCLE('',#13401,0.164999999999999);
#4719=CIRCLE('',#13402,0.164999999999999);
#4720=CIRCLE('',#13404,0.164999999999999);
#4721=CIRCLE('',#13405,0.164999999999999);
#4722=CIRCLE('',#13407,1.6);
#4723=CIRCLE('',#13408,1.6);
#4724=CIRCLE('',#13410,0.525);
#4725=CIRCLE('',#13412,0.525);
#4726=CIRCLE('',#13414,0.525);
#4727=CIRCLE('',#13416,0.525);
#4728=CIRCLE('',#13418,0.525);
#4729=CIRCLE('',#13420,0.525);
#4730=CIRCLE('',#13422,0.525);
#4731=CIRCLE('',#13424,0.525);
#4732=CIRCLE('',#13428,0.225);
#4733=CIRCLE('',#13429,0.225);
#4734=CIRCLE('',#13431,0.225);
#4735=CIRCLE('',#13432,0.225);
#4736=CIRCLE('',#13434,0.225);
#4737=CIRCLE('',#13435,0.225);
#4738=CIRCLE('',#13437,0.225);
#4739=CIRCLE('',#13438,0.225);
#4740=CIRCLE('',#13449,1.2);
#4741=CIRCLE('',#13450,1.2);
#4742=CIRCLE('',#13452,1.59);
#4743=CIRCLE('',#13453,1.59);
#4744=CIRCLE('',#13458,0.225);
#4745=CIRCLE('',#13459,0.225);
#4746=CIRCLE('',#13461,0.225);
#4747=CIRCLE('',#13462,0.225);
#4748=CIRCLE('',#13464,0.225);
#4749=CIRCLE('',#13465,0.225);
#4750=CIRCLE('',#13467,0.225);
#4751=CIRCLE('',#13468,0.225);
#4752=CIRCLE('',#13470,2.2);
#4753=CIRCLE('',#13471,2.2);
#4754=CIRCLE('',#13472,2.2);
#4755=CIRCLE('',#13473,2.2);
#4756=CIRCLE('',#13474,1.2);
#4757=CIRCLE('',#13476,2.2);
#4758=CIRCLE('',#13478,2.2);
#4759=CIRCLE('',#13480,2.2);
#4760=CIRCLE('',#13482,2.2);
#4761=CIRCLE('',#13484,1.59);
#4762=CIRCLE('',#13485,1.59);
#4763=CIRCLE('',#13487,1.2);
#4764=CIRCLE('',#13492,0.225);
#4765=CIRCLE('',#13493,0.225);
#4766=CIRCLE('',#13495,0.225);
#4767=CIRCLE('',#13496,0.225);
#4768=CIRCLE('',#13498,0.225);
#4769=CIRCLE('',#13499,0.225);
#4770=CIRCLE('',#13501,0.225);
#4771=CIRCLE('',#13502,0.225);
#4772=CIRCLE('',#13504,2.2);
#4773=CIRCLE('',#13505,2.2);
#4774=CIRCLE('',#13506,2.2);
#4775=CIRCLE('',#13507,2.2);
#4776=CIRCLE('',#13508,1.59);
#4777=CIRCLE('',#13510,2.2);
#4778=CIRCLE('',#13512,2.2);
#4779=CIRCLE('',#13514,2.2);
#4780=CIRCLE('',#13516,2.2);
#4781=CIRCLE('',#13518,1.59);
#4782=CIRCLE('',#13520,1.2);
#4783=CIRCLE('',#13522,1.2);
#4784=CIRCLE('',#13526,0.164999999999999);
#4785=CIRCLE('',#13527,0.164999999999999);
#4786=CIRCLE('',#13530,0.164999999999999);
#4787=CIRCLE('',#13531,0.164999999999999);
#4788=CIRCLE('',#13534,0.34);
#4789=CIRCLE('',#13535,0.34);
#4790=CIRCLE('',#13544,0.3);
#4791=CIRCLE('',#13546,0.3);
#4792=CIRCLE('',#13550,0.164999999999999);
#4793=CIRCLE('',#13552,0.164999999999999);
#4794=CIRCLE('',#13553,0.164999999999999);
#4795=CIRCLE('',#13556,0.3);
#4796=CIRCLE('',#13557,0.3);
#4797=CIRCLE('',#13567,0.21);
#4798=CIRCLE('',#13569,0.21);
#4799=CIRCLE('',#13570,0.21);
#4800=CIRCLE('',#13571,0.21);
#4801=CIRCLE('',#13573,0.21);
#4802=CIRCLE('',#13575,0.21);
#4803=CIRCLE('',#13576,0.21);
#4804=CIRCLE('',#13577,0.21);
#4805=CIRCLE('',#13579,0.21);
#4806=CIRCLE('',#13581,0.21);
#4807=CIRCLE('',#13582,0.21);
#4808=CIRCLE('',#13583,0.21);
#4809=CIRCLE('',#13585,0.21);
#4810=CIRCLE('',#13587,0.21);
#4811=CIRCLE('',#13588,0.21);
#4812=CIRCLE('',#13589,0.21);
#4813=CIRCLE('',#13639,0.24505);
#4814=CIRCLE('',#13641,0.375);
#4815=CIRCLE('',#13643,0.425);
#4816=CIRCLE('',#13645,0.425);
#4817=CIRCLE('',#13647,0.395);
#4818=CIRCLE('',#13649,0.27);
#4819=CIRCLE('',#13651,0.24505);
#4820=CIRCLE('',#13656,1.070235);
#4821=CIRCLE('',#13657,1.070235);
#4822=CIRCLE('',#13658,0.309556);
#4823=CIRCLE('',#13659,1.070235);
#4824=CIRCLE('',#13660,1.070235);
#4825=CIRCLE('',#13662,1.070235);
#4826=CIRCLE('',#13664,0.6);
#4827=CIRCLE('',#13665,0.6);
#4828=CIRCLE('',#13667,0.66);
#4829=CIRCLE('',#13670,1.070235);
#4830=CIRCLE('',#13672,0.66);
#4831=CIRCLE('',#13676,1.129765);
#4832=CIRCLE('',#13677,1.129765);
#4833=CIRCLE('',#13678,0.309556);
#4834=CIRCLE('',#13679,1.129765);
#4835=CIRCLE('',#13680,1.129765);
#4836=CIRCLE('',#13682,1.129765);
#4837=CIRCLE('',#13684,1.54);
#4838=CIRCLE('',#13685,1.129765);
#4839=CIRCLE('',#13687,1.6);
#4840=CIRCLE('',#13689,1.6);
#4841=CIRCLE('',#13691,1.54);
#4842=CIRCLE('',#13696,0.29765);
#4843=CIRCLE('',#13698,0.29765);
#4844=CIRCLE('',#13700,0.29765);
#4845=CIRCLE('',#13702,0.29765);
#4846=CIRCLE('',#13704,0.29765);
#4847=CIRCLE('',#13706,0.29765);
#4848=CIRCLE('',#13708,0.29765);
#4849=CIRCLE('',#13711,0.303778037777585);
#4850=CIRCLE('',#13712,0.303778037777585);
#4851=CIRCLE('',#13714,1.123812);
#4852=CIRCLE('',#13715,1.123812);
#4853=CIRCLE('',#13716,1.123812);
#4854=CIRCLE('',#13717,1.123812);
#4855=CIRCLE('',#13718,1.123812);
#4856=CIRCLE('',#13719,1.123812);
#4857=CIRCLE('',#13720,1.123812);
#4858=CIRCLE('',#13721,1.123812);
#4859=CIRCLE('',#13722,1.123812);
#4860=CIRCLE('',#13724,1.076188);
#4861=CIRCLE('',#13725,0.303778037777585);
#4862=CIRCLE('',#13727,0.303778037777585);
#4863=CIRCLE('',#13729,1.076188);
#4864=CIRCLE('',#13730,0.303778037777585);
#4865=CIRCLE('',#13732,0.303778037777585);
#4866=CIRCLE('',#13734,1.076188);
#4867=CIRCLE('',#13735,1.076188);
#4868=CIRCLE('',#13736,0.303778037777585);
#4869=CIRCLE('',#13738,0.303778037777585);
#4870=CIRCLE('',#13740,1.076188);
#4871=CIRCLE('',#13741,0.303778037777585);
#4872=CIRCLE('',#13743,0.303778037777585);
#4873=CIRCLE('',#13745,1.076188);
#4874=CIRCLE('',#13746,0.303778037777585);
#4875=CIRCLE('',#13748,0.303778037777585);
#4876=CIRCLE('',#13750,1.076188);
#4877=CIRCLE('',#13751,1.076188);
#4878=CIRCLE('',#13752,1.076188);
#4879=CIRCLE('',#13754,0.303778037777585);
#4880=CIRCLE('',#13756,0.303778037777585);
#4881=CIRCLE('',#13761,1.119765);
#4882=CIRCLE('',#13762,1.085235);
#4883=CIRCLE('',#13764,1.119765);
#4884=CIRCLE('',#13766,1.085235);
#4885=CIRCLE('',#13769,1.119765);
#4886=CIRCLE('',#13770,1.085235);
#4887=CIRCLE('',#13772,1.119765);
#4888=CIRCLE('',#13774,1.085235);
#4889=CIRCLE('',#13791,0.1954);
#4890=CIRCLE('',#13793,0.3);
#4891=CIRCLE('',#13795,0.35);
#4892=CIRCLE('',#13797,0.35);
#4893=CIRCLE('',#13799,0.32);
#4894=CIRCLE('',#13801,0.22);
#4895=CIRCLE('',#13803,0.1954);
#4896=CIRCLE('',#13808,0.165);
#4897=CIRCLE('',#13809,0.165);
#4898=CIRCLE('',#13812,0.7);
#4899=CIRCLE('',#13813,0.5);
#4900=CIRCLE('',#13815,0.7);
#4901=CIRCLE('',#13816,0.5);
#4902=CIRCLE('',#13819,0.5);
#4903=CIRCLE('',#13821,0.4);
#4904=CIRCLE('',#13822,0.4);
#4905=CIRCLE('',#13825,0.5);
#4906=CIRCLE('',#13830,0.505);
#4907=CIRCLE('',#13831,0.505);
#4908=CIRCLE('',#13833,0.405);
#4909=CIRCLE('',#13835,0.405);
#4910=CIRCLE('',#13837,0.7);
#4911=CIRCLE('',#13838,0.7);
#4912=CIRCLE('',#13843,0.505);
#4913=CIRCLE('',#13844,0.505);
#4914=CIRCLE('',#13846,0.7);
#4915=CIRCLE('',#13847,0.7);
#4916=CIRCLE('',#13852,0.15);
#4917=CIRCLE('',#13853,0.15);
#4918=CIRCLE('',#13858,0.15);
#4919=CIRCLE('',#13859,0.15);
#4920=CIRCLE('',#13864,0.225);
#4921=CIRCLE('',#13865,0.225);
#4922=CIRCLE('',#13867,0.6);
#4923=CIRCLE('',#13868,0.6);
#4924=CIRCLE('',#13875,0.65);
#4925=CIRCLE('',#13876,0.65);
#4926=CIRCLE('',#13880,0.4);
#4927=CIRCLE('',#13881,0.4);
#4928=CIRCLE('',#13884,0.8);
#4929=CIRCLE('',#13885,0.0555);
#4930=CIRCLE('',#13886,0.611219772367581);
#4931=CIRCLE('',#13887,0.0555);
#4932=CIRCLE('',#13888,0.611219772367581);
#4933=CIRCLE('',#13889,0.0555);
#4934=CIRCLE('',#13890,0.611219772367581);
#4935=CIRCLE('',#13891,0.0555);
#4936=CIRCLE('',#13892,0.611219772367581);
#4937=CIRCLE('',#13893,0.0555);
#4938=CIRCLE('',#13894,0.611219772367581);
#4939=CIRCLE('',#13895,0.0555);
#4940=CIRCLE('',#13896,0.611219772367581);
#4941=CIRCLE('',#13897,0.0555);
#4942=CIRCLE('',#13898,0.611219772367581);
#4943=CIRCLE('',#13899,0.0555);
#4944=CIRCLE('',#13900,0.611219772367581);
#4945=CIRCLE('',#13901,0.0555);
#4946=CIRCLE('',#13902,0.611219772367581);
#4947=CIRCLE('',#13903,0.0555);
#4948=CIRCLE('',#13904,0.611219772367581);
#4949=CIRCLE('',#13905,0.0555);
#4950=CIRCLE('',#13906,0.611219772367581);
#4951=CIRCLE('',#13907,0.0555);
#4952=CIRCLE('',#13908,0.611219772367581);
#4953=CIRCLE('',#13909,0.0555);
#4954=CIRCLE('',#13910,0.611219772367581);
#4955=CIRCLE('',#13911,0.0555);
#4956=CIRCLE('',#13912,0.611219772367581);
#4957=CIRCLE('',#13913,0.0555);
#4958=CIRCLE('',#13914,0.611219772367581);
#4959=CIRCLE('',#13915,0.0555);
#4960=CIRCLE('',#13916,0.611219772367581);
#4961=CIRCLE('',#13917,0.0555);
#4962=CIRCLE('',#13918,0.611219772367581);
#4963=CIRCLE('',#13919,0.0555);
#4964=CIRCLE('',#13920,0.611219772367581);
#4965=CIRCLE('',#13921,0.0555);
#4966=CIRCLE('',#13922,0.611219772367581);
#4967=CIRCLE('',#13923,0.0555);
#4968=CIRCLE('',#13924,0.611219772367581);
#4969=CIRCLE('',#13926,0.8);
#4970=CIRCLE('',#13929,0.8);
#4971=CIRCLE('',#13930,0.0555);
#4972=CIRCLE('',#13931,0.611219772367581);
#4973=CIRCLE('',#13932,0.0555);
#4974=CIRCLE('',#13933,0.611219772367581);
#4975=CIRCLE('',#13934,0.0555);
#4976=CIRCLE('',#13935,0.611219772367581);
#4977=CIRCLE('',#13936,0.0555);
#4978=CIRCLE('',#13937,0.611219772367581);
#4979=CIRCLE('',#13938,0.0555);
#4980=CIRCLE('',#13939,0.611219772367581);
#4981=CIRCLE('',#13940,0.0555);
#4982=CIRCLE('',#13941,0.611219772367581);
#4983=CIRCLE('',#13942,0.0555);
#4984=CIRCLE('',#13943,0.611219772367581);
#4985=CIRCLE('',#13944,0.0555);
#4986=CIRCLE('',#13945,0.611219772367581);
#4987=CIRCLE('',#13946,0.0555);
#4988=CIRCLE('',#13947,0.611219772367581);
#4989=CIRCLE('',#13948,0.0555);
#4990=CIRCLE('',#13949,0.611219772367581);
#4991=CIRCLE('',#13950,0.0555);
#4992=CIRCLE('',#13951,0.611219772367581);
#4993=CIRCLE('',#13952,0.0555);
#4994=CIRCLE('',#13953,0.611219772367581);
#4995=CIRCLE('',#13954,0.0555);
#4996=CIRCLE('',#13955,0.611219772367581);
#4997=CIRCLE('',#13956,0.0555);
#4998=CIRCLE('',#13957,0.611219772367581);
#4999=CIRCLE('',#13958,0.0555);
#5000=CIRCLE('',#13959,0.611219772367581);
#5001=CIRCLE('',#13960,0.0555);
#5002=CIRCLE('',#13961,0.611219772367581);
#5003=CIRCLE('',#13962,0.0555);
#5004=CIRCLE('',#13963,0.611219772367581);
#5005=CIRCLE('',#13964,0.0555);
#5006=CIRCLE('',#13965,0.611219772367581);
#5007=CIRCLE('',#13966,0.0555);
#5008=CIRCLE('',#13967,0.611219772367581);
#5009=CIRCLE('',#13968,0.0555);
#5010=CIRCLE('',#13969,0.611219772367581);
#5011=CIRCLE('',#13971,0.8);
#5012=CIRCLE('',#14016,0.164999999999999);
#5013=CIRCLE('',#14017,0.164999999999999);
#5014=CIRCLE('',#14020,0.800000000000001);
#5015=CIRCLE('',#14021,0.6);
#5016=CIRCLE('',#14023,0.800000000000001);
#5017=CIRCLE('',#14024,0.6);
#5018=CIRCLE('',#14027,0.6);
#5019=CIRCLE('',#14030,0.6);
#5020=CIRCLE('',#14034,0.605);
#5021=CIRCLE('',#14035,0.605);
#5022=CIRCLE('',#14037,0.800000000000001);
#5023=CIRCLE('',#14038,0.800000000000001);
#5024=CIRCLE('',#14043,0.605);
#5025=CIRCLE('',#14044,0.605);
#5026=CIRCLE('',#14046,0.800000000000001);
#5027=CIRCLE('',#14047,0.800000000000001);
#5028=CIRCLE('',#14052,0.15);
#5029=CIRCLE('',#14053,0.15);
#5030=CIRCLE('',#14058,0.15);
#5031=CIRCLE('',#14059,0.15);
#5032=CIRCLE('',#14064,0.225);
#5033=CIRCLE('',#14065,0.225);
#5034=CIRCLE('',#14067,0.800000000000001);
#5035=CIRCLE('',#14068,0.800000000000001);
#5036=CIRCLE('',#14075,1.);
#5037=CIRCLE('',#14076,1.);
#5038=CIRCLE('',#14080,0.6);
#5039=CIRCLE('',#14081,0.6);
#5040=CIRCLE('',#14084,1.4);
#5041=CIRCLE('',#14085,0.0555000000000001);
#5042=CIRCLE('',#14086,1.24783954473516);
#5043=CIRCLE('',#14087,0.0555000000000001);
#5044=CIRCLE('',#14088,1.24783954473516);
#5045=CIRCLE('',#14089,0.0555000000000001);
#5046=CIRCLE('',#14090,1.24783954473516);
#5047=CIRCLE('',#14091,0.0555000000000001);
#5048=CIRCLE('',#14092,1.24783954473516);
#5049=CIRCLE('',#14093,0.0555000000000001);
#5050=CIRCLE('',#14094,1.24783954473516);
#5051=CIRCLE('',#14095,0.0555000000000001);
#5052=CIRCLE('',#14096,1.24783954473516);
#5053=CIRCLE('',#14097,0.0555000000000001);
#5054=CIRCLE('',#14098,1.24783954473516);
#5055=CIRCLE('',#14099,0.0555000000000001);
#5056=CIRCLE('',#14100,1.24783954473516);
#5057=CIRCLE('',#14101,0.0555000000000001);
#5058=CIRCLE('',#14102,1.24783954473516);
#5059=CIRCLE('',#14103,0.0555000000000001);
#5060=CIRCLE('',#14104,1.24783954473516);
#5061=CIRCLE('',#14105,0.0555000000000001);
#5062=CIRCLE('',#14106,1.24783954473516);
#5063=CIRCLE('',#14107,0.0555000000000001);
#5064=CIRCLE('',#14108,1.24783954473516);
#5065=CIRCLE('',#14109,0.0555000000000001);
#5066=CIRCLE('',#14110,1.24783954473516);
#5067=CIRCLE('',#14111,0.0555000000000001);
#5068=CIRCLE('',#14112,1.24783954473516);
#5069=CIRCLE('',#14113,0.0555000000000001);
#5070=CIRCLE('',#14114,1.24783954473516);
#5071=CIRCLE('',#14115,0.0555000000000001);
#5072=CIRCLE('',#14116,1.24783954473516);
#5073=CIRCLE('',#14117,0.0555000000000001);
#5074=CIRCLE('',#14118,1.24783954473516);
#5075=CIRCLE('',#14119,0.0555000000000001);
#5076=CIRCLE('',#14120,1.24783954473516);
#5077=CIRCLE('',#14121,0.0555000000000001);
#5078=CIRCLE('',#14122,1.24783954473516);
#5079=CIRCLE('',#14123,0.0555000000000001);
#5080=CIRCLE('',#14124,1.24783954473516);
#5081=CIRCLE('',#14125,0.0555000000000001);
#5082=CIRCLE('',#14126,1.24783954473516);
#5083=CIRCLE('',#14127,0.0555000000000001);
#5084=CIRCLE('',#14128,1.24783954473516);
#5085=CIRCLE('',#14129,0.0555000000000001);
#5086=CIRCLE('',#14130,1.24783954473516);
#5087=CIRCLE('',#14131,0.0555000000000001);
#5088=CIRCLE('',#14132,1.24783954473516);
#5089=CIRCLE('',#14133,0.0555000000000001);
#5090=CIRCLE('',#14134,1.24783954473516);
#5091=CIRCLE('',#14135,0.0555000000000001);
#5092=CIRCLE('',#14136,1.24783954473516);
#5093=CIRCLE('',#14137,0.0555000000000001);
#5094=CIRCLE('',#14138,1.24783954473516);
#5095=CIRCLE('',#14139,0.0555000000000001);
#5096=CIRCLE('',#14140,1.24783954473516);
#5097=CIRCLE('',#14141,0.0555000000000001);
#5098=CIRCLE('',#14142,1.24783954473516);
#5099=CIRCLE('',#14143,0.0555000000000001);
#5100=CIRCLE('',#14144,1.24783954473516);
#5101=CIRCLE('',#14145,0.0555000000000001);
#5102=CIRCLE('',#14146,1.24783954473516);
#5103=CIRCLE('',#14147,0.0555000000000001);
#5104=CIRCLE('',#14148,1.24783954473516);
#5105=CIRCLE('',#14149,0.0555000000000001);
#5106=CIRCLE('',#14150,1.24783954473516);
#5107=CIRCLE('',#14151,0.0555000000000001);
#5108=CIRCLE('',#14152,1.24783954473516);
#5109=CIRCLE('',#14153,0.0555000000000001);
#5110=CIRCLE('',#14154,1.24783954473516);
#5111=CIRCLE('',#14155,0.0555000000000001);
#5112=CIRCLE('',#14156,1.24783954473516);
#5113=CIRCLE('',#14157,0.0555000000000001);
#5114=CIRCLE('',#14158,1.24783954473516);
#5115=CIRCLE('',#14159,0.0555000000000001);
#5116=CIRCLE('',#14160,1.24783954473516);
#5117=CIRCLE('',#14161,0.0555000000000001);
#5118=CIRCLE('',#14162,1.24783954473516);
#5119=CIRCLE('',#14163,0.0555000000000001);
#5120=CIRCLE('',#14164,1.24783954473516);
#5121=CIRCLE('',#14166,1.4);
#5122=CIRCLE('',#14169,1.4);
#5123=CIRCLE('',#14170,0.0555000000000001);
#5124=CIRCLE('',#14171,1.24783954473516);
#5125=CIRCLE('',#14172,0.0555000000000001);
#5126=CIRCLE('',#14173,1.24783954473516);
#5127=CIRCLE('',#14174,0.0555000000000001);
#5128=CIRCLE('',#14175,1.24783954473516);
#5129=CIRCLE('',#14176,0.0555000000000001);
#5130=CIRCLE('',#14177,1.24783954473516);
#5131=CIRCLE('',#14178,0.0555000000000001);
#5132=CIRCLE('',#14179,1.24783954473516);
#5133=CIRCLE('',#14180,0.0555000000000001);
#5134=CIRCLE('',#14181,1.24783954473516);
#5135=CIRCLE('',#14182,0.0555000000000001);
#5136=CIRCLE('',#14183,1.24783954473516);
#5137=CIRCLE('',#14184,0.0555000000000001);
#5138=CIRCLE('',#14185,1.24783954473516);
#5139=CIRCLE('',#14186,0.0555000000000001);
#5140=CIRCLE('',#14187,1.24783954473516);
#5141=CIRCLE('',#14188,0.0555000000000001);
#5142=CIRCLE('',#14189,1.24783954473516);
#5143=CIRCLE('',#14190,0.0555000000000001);
#5144=CIRCLE('',#14191,1.24783954473516);
#5145=CIRCLE('',#14192,0.0555000000000001);
#5146=CIRCLE('',#14193,1.24783954473516);
#5147=CIRCLE('',#14194,0.0555000000000001);
#5148=CIRCLE('',#14195,1.24783954473516);
#5149=CIRCLE('',#14196,0.0555000000000001);
#5150=CIRCLE('',#14197,1.24783954473516);
#5151=CIRCLE('',#14198,0.0555000000000001);
#5152=CIRCLE('',#14199,1.24783954473516);
#5153=CIRCLE('',#14200,0.0555000000000001);
#5154=CIRCLE('',#14201,1.24783954473516);
#5155=CIRCLE('',#14202,0.0555000000000001);
#5156=CIRCLE('',#14203,1.24783954473516);
#5157=CIRCLE('',#14204,0.0555000000000001);
#5158=CIRCLE('',#14205,1.24783954473516);
#5159=CIRCLE('',#14206,0.0555000000000001);
#5160=CIRCLE('',#14207,1.24783954473516);
#5161=CIRCLE('',#14208,0.0555000000000001);
#5162=CIRCLE('',#14209,1.24783954473516);
#5163=CIRCLE('',#14210,0.0555000000000001);
#5164=CIRCLE('',#14211,1.24783954473516);
#5165=CIRCLE('',#14212,0.0555000000000001);
#5166=CIRCLE('',#14213,1.24783954473516);
#5167=CIRCLE('',#14214,0.0555000000000001);
#5168=CIRCLE('',#14215,1.24783954473516);
#5169=CIRCLE('',#14216,0.0555000000000001);
#5170=CIRCLE('',#14217,1.24783954473516);
#5171=CIRCLE('',#14218,0.0555000000000001);
#5172=CIRCLE('',#14219,1.24783954473516);
#5173=CIRCLE('',#14220,0.0555000000000001);
#5174=CIRCLE('',#14221,1.24783954473516);
#5175=CIRCLE('',#14222,0.0555000000000001);
#5176=CIRCLE('',#14223,1.24783954473516);
#5177=CIRCLE('',#14224,0.0555000000000001);
#5178=CIRCLE('',#14225,1.24783954473516);
#5179=CIRCLE('',#14226,0.0555000000000001);
#5180=CIRCLE('',#14227,1.24783954473516);
#5181=CIRCLE('',#14228,0.0555000000000001);
#5182=CIRCLE('',#14229,1.24783954473516);
#5183=CIRCLE('',#14230,0.0555000000000001);
#5184=CIRCLE('',#14231,1.24783954473516);
#5185=CIRCLE('',#14232,0.0555000000000001);
#5186=CIRCLE('',#14233,1.24783954473516);
#5187=CIRCLE('',#14234,0.0555000000000001);
#5188=CIRCLE('',#14235,1.24783954473516);
#5189=CIRCLE('',#14236,0.0555000000000001);
#5190=CIRCLE('',#14237,1.24783954473516);
#5191=CIRCLE('',#14238,0.0555000000000001);
#5192=CIRCLE('',#14239,1.24783954473516);
#5193=CIRCLE('',#14240,0.0555000000000001);
#5194=CIRCLE('',#14241,1.24783954473516);
#5195=CIRCLE('',#14242,0.0555000000000001);
#5196=CIRCLE('',#14243,1.24783954473516);
#5197=CIRCLE('',#14244,0.0555000000000001);
#5198=CIRCLE('',#14245,1.24783954473516);
#5199=CIRCLE('',#14246,0.0555000000000001);
#5200=CIRCLE('',#14247,1.24783954473516);
#5201=CIRCLE('',#14248,0.0555000000000001);
#5202=CIRCLE('',#14249,1.24783954473516);
#5203=CIRCLE('',#14251,1.4);
#5204=CIRCLE('',#14335,0.3);
#5205=CIRCLE('',#14337,0.35);
#5206=CIRCLE('',#14339,0.35);
#5207=CIRCLE('',#14341,0.32);
#5208=CIRCLE('',#14343,0.22);
#5209=CIRCLE('',#14345,0.1954);
#5210=CIRCLE('',#14347,0.1954);
#5211=CIRCLE('',#14349,0.16);
#5212=CIRCLE('',#14416,0.4);
#5213=CIRCLE('',#14417,0.4);
#5214=CIRCLE('',#14420,0.9);
#5215=CIRCLE('',#14421,0.6);
#5216=CIRCLE('',#14423,0.9);
#5217=CIRCLE('',#14424,0.6);
#5218=CIRCLE('',#14427,0.6);
#5219=CIRCLE('',#14429,0.9);
#5220=CIRCLE('',#14430,0.6);
#5221=CIRCLE('',#14432,0.9);
#5222=CIRCLE('',#14433,0.6);
#5223=CIRCLE('',#14436,0.6);
#5224=CIRCLE('',#14438,0.4);
#5225=CIRCLE('',#14440,0.6);
#5226=CIRCLE('',#14442,0.6);
#5227=CIRCLE('',#14443,0.4);
#5228=CIRCLE('',#14450,0.165);
#5229=CIRCLE('',#14452,0.165);
#5230=CIRCLE('',#14455,0.4);
#5231=CIRCLE('',#14456,0.4);
#5232=CIRCLE('',#14458,1.5);
#5233=CIRCLE('',#14459,1.5);
#5234=CIRCLE('',#14471,0.17);
#5235=CIRCLE('',#14473,0.1954);
#5236=CIRCLE('',#14475,0.1954);
#5237=CIRCLE('',#14477,0.125);
#5238=VERTEX_POINT('',#18554);
#5239=VERTEX_POINT('',#18556);
#5240=VERTEX_POINT('',#18561);
#5241=VERTEX_POINT('',#18563);
#5242=VERTEX_POINT('',#18568);
#5243=VERTEX_POINT('',#18570);
#5244=VERTEX_POINT('',#18575);
#5245=VERTEX_POINT('',#18577);
#5246=VERTEX_POINT('',#18582);
#5247=VERTEX_POINT('',#18584);
#5248=VERTEX_POINT('',#18589);
#5249=VERTEX_POINT('',#18591);
#5250=VERTEX_POINT('',#18596);
#5251=VERTEX_POINT('',#18598);
#5252=VERTEX_POINT('',#18603);
#5253=VERTEX_POINT('',#18605);
#5254=VERTEX_POINT('',#18610);
#5255=VERTEX_POINT('',#18612);
#5256=VERTEX_POINT('',#18617);
#5257=VERTEX_POINT('',#18619);
#5258=VERTEX_POINT('',#18624);
#5259=VERTEX_POINT('',#18626);
#5260=VERTEX_POINT('',#18631);
#5261=VERTEX_POINT('',#18633);
#5262=VERTEX_POINT('',#18638);
#5263=VERTEX_POINT('',#18640);
#5264=VERTEX_POINT('',#18645);
#5265=VERTEX_POINT('',#18647);
#5266=VERTEX_POINT('',#18652);
#5267=VERTEX_POINT('',#18653);
#5268=VERTEX_POINT('',#18655);
#5269=VERTEX_POINT('',#18657);
#5270=VERTEX_POINT('',#18661);
#5271=VERTEX_POINT('',#18663);
#5272=VERTEX_POINT('',#18667);
#5273=VERTEX_POINT('',#18669);
#5274=VERTEX_POINT('',#18679);
#5275=VERTEX_POINT('',#18680);
#5276=VERTEX_POINT('',#18682);
#5277=VERTEX_POINT('',#18684);
#5278=VERTEX_POINT('',#18688);
#5279=VERTEX_POINT('',#18690);
#5280=VERTEX_POINT('',#18694);
#5281=VERTEX_POINT('',#18696);
#5282=VERTEX_POINT('',#18706);
#5283=VERTEX_POINT('',#18707);
#5284=VERTEX_POINT('',#18709);
#5285=VERTEX_POINT('',#18711);
#5286=VERTEX_POINT('',#18715);
#5287=VERTEX_POINT('',#18717);
#5288=VERTEX_POINT('',#18721);
#5289=VERTEX_POINT('',#18723);
#5290=VERTEX_POINT('',#18733);
#5291=VERTEX_POINT('',#18735);
#5292=VERTEX_POINT('',#18739);
#5293=VERTEX_POINT('',#18741);
#5294=VERTEX_POINT('',#18745);
#5295=VERTEX_POINT('',#18747);
#5296=VERTEX_POINT('',#18751);
#5297=VERTEX_POINT('',#18753);
#5298=VERTEX_POINT('',#18757);
#5299=VERTEX_POINT('',#18759);
#5300=VERTEX_POINT('',#18763);
#5301=VERTEX_POINT('',#18765);
#5302=VERTEX_POINT('',#18769);
#5303=VERTEX_POINT('',#18771);
#5304=VERTEX_POINT('',#18775);
#5305=VERTEX_POINT('',#18777);
#5306=VERTEX_POINT('',#18781);
#5307=VERTEX_POINT('',#18783);
#5308=VERTEX_POINT('',#18787);
#5309=VERTEX_POINT('',#18788);
#5310=VERTEX_POINT('',#18790);
#5311=VERTEX_POINT('',#18792);
#5312=VERTEX_POINT('',#18796);
#5313=VERTEX_POINT('',#18797);
#5314=VERTEX_POINT('',#18799);
#5315=VERTEX_POINT('',#18801);
#5316=VERTEX_POINT('',#18805);
#5317=VERTEX_POINT('',#18807);
#5318=VERTEX_POINT('',#18811);
#5319=VERTEX_POINT('',#18813);
#5320=VERTEX_POINT('',#18817);
#5321=VERTEX_POINT('',#18819);
#5322=VERTEX_POINT('',#18824);
#5323=VERTEX_POINT('',#18828);
#5324=VERTEX_POINT('',#18838);
#5325=VERTEX_POINT('',#18840);
#5326=VERTEX_POINT('',#18844);
#5327=VERTEX_POINT('',#18846);
#5328=VERTEX_POINT('',#18853);
#5329=VERTEX_POINT('',#18854);
#5330=VERTEX_POINT('',#18856);
#5331=VERTEX_POINT('',#18858);
#5332=VERTEX_POINT('',#18862);
#5333=VERTEX_POINT('',#18863);
#5334=VERTEX_POINT('',#18865);
#5335=VERTEX_POINT('',#18867);
#5336=VERTEX_POINT('',#18871);
#5337=VERTEX_POINT('',#18872);
#5338=VERTEX_POINT('',#18874);
#5339=VERTEX_POINT('',#18876);
#5340=VERTEX_POINT('',#18880);
#5341=VERTEX_POINT('',#18881);
#5342=VERTEX_POINT('',#18883);
#5343=VERTEX_POINT('',#18885);
#5344=VERTEX_POINT('',#18893);
#5345=VERTEX_POINT('',#18904);
#5346=VERTEX_POINT('',#18906);
#5347=VERTEX_POINT('',#18910);
#5348=VERTEX_POINT('',#18917);
#5349=VERTEX_POINT('',#18918);
#5350=VERTEX_POINT('',#18920);
#5351=VERTEX_POINT('',#18922);
#5352=VERTEX_POINT('',#18926);
#5353=VERTEX_POINT('',#18927);
#5354=VERTEX_POINT('',#18929);
#5355=VERTEX_POINT('',#18931);
#5356=VERTEX_POINT('',#18935);
#5357=VERTEX_POINT('',#18936);
#5358=VERTEX_POINT('',#18938);
#5359=VERTEX_POINT('',#18940);
#5360=VERTEX_POINT('',#18944);
#5361=VERTEX_POINT('',#18945);
#5362=VERTEX_POINT('',#18947);
#5363=VERTEX_POINT('',#18949);
#5364=VERTEX_POINT('',#18957);
#5365=VERTEX_POINT('',#18968);
#5366=VERTEX_POINT('',#18972);
#5367=VERTEX_POINT('',#18975);
#5368=VERTEX_POINT('',#18981);
#5369=VERTEX_POINT('',#18983);
#5370=VERTEX_POINT('',#18987);
#5371=VERTEX_POINT('',#18990);
#5372=VERTEX_POINT('',#18992);
#5373=VERTEX_POINT('',#18996);
#5374=VERTEX_POINT('',#18999);
#5375=VERTEX_POINT('',#19003);
#5376=VERTEX_POINT('',#19007);
#5377=VERTEX_POINT('',#19009);
#5378=VERTEX_POINT('',#19013);
#5379=VERTEX_POINT('',#19014);
#5380=VERTEX_POINT('',#19016);
#5381=VERTEX_POINT('',#19018);
#5382=VERTEX_POINT('',#19022);
#5383=VERTEX_POINT('',#19024);
#5384=VERTEX_POINT('',#19028);
#5385=VERTEX_POINT('',#19030);
#5386=VERTEX_POINT('',#19040);
#5387=VERTEX_POINT('',#19042);
#5388=VERTEX_POINT('',#19046);
#5389=VERTEX_POINT('',#19048);
#5390=VERTEX_POINT('',#19055);
#5391=VERTEX_POINT('',#19057);
#5392=VERTEX_POINT('',#19061);
#5393=VERTEX_POINT('',#19064);
#5394=VERTEX_POINT('',#19066);
#5395=VERTEX_POINT('',#19070);
#5396=VERTEX_POINT('',#19073);
#5397=VERTEX_POINT('',#19077);
#5398=VERTEX_POINT('',#19081);
#5399=VERTEX_POINT('',#19083);
#5400=VERTEX_POINT('',#19087);
#5401=VERTEX_POINT('',#19088);
#5402=VERTEX_POINT('',#19090);
#5403=VERTEX_POINT('',#19092);
#5404=VERTEX_POINT('',#19096);
#5405=VERTEX_POINT('',#19098);
#5406=VERTEX_POINT('',#19102);
#5407=VERTEX_POINT('',#19104);
#5408=VERTEX_POINT('',#19114);
#5409=VERTEX_POINT('',#19116);
#5410=VERTEX_POINT('',#19120);
#5411=VERTEX_POINT('',#19122);
#5412=VERTEX_POINT('',#19129);
#5413=VERTEX_POINT('',#19131);
#5414=VERTEX_POINT('',#19135);
#5415=VERTEX_POINT('',#19137);
#5416=VERTEX_POINT('',#19144);
#5417=VERTEX_POINT('',#19145);
#5418=VERTEX_POINT('',#19147);
#5419=VERTEX_POINT('',#19149);
#5420=VERTEX_POINT('',#19151);
#5421=VERTEX_POINT('',#19160);
#5422=VERTEX_POINT('',#19161);
#5423=VERTEX_POINT('',#19163);
#5424=VERTEX_POINT('',#19165);
#5425=VERTEX_POINT('',#19167);
#5426=VERTEX_POINT('',#19202);
#5427=VERTEX_POINT('',#19213);
#5428=VERTEX_POINT('',#19216);
#5429=VERTEX_POINT('',#19253);
#5430=VERTEX_POINT('',#19256);
#5431=VERTEX_POINT('',#19258);
#5432=VERTEX_POINT('',#19262);
#5433=VERTEX_POINT('',#19264);
#5434=VERTEX_POINT('',#19268);
#5435=VERTEX_POINT('',#19270);
#5436=VERTEX_POINT('',#19274);
#5437=VERTEX_POINT('',#19278);
#5438=VERTEX_POINT('',#19282);
#5439=VERTEX_POINT('',#19287);
#5440=VERTEX_POINT('',#19289);
#5441=VERTEX_POINT('',#19291);
#5442=VERTEX_POINT('',#19297);
#5443=VERTEX_POINT('',#19301);
#5444=VERTEX_POINT('',#19309);
#5445=VERTEX_POINT('',#19311);
#5446=VERTEX_POINT('',#19315);
#5447=VERTEX_POINT('',#19318);
#5448=VERTEX_POINT('',#19320);
#5449=VERTEX_POINT('',#19324);
#5450=VERTEX_POINT('',#19327);
#5451=VERTEX_POINT('',#19329);
#5452=VERTEX_POINT('',#19333);
#5453=VERTEX_POINT('',#19336);
#5454=VERTEX_POINT('',#19338);
#5455=VERTEX_POINT('',#19342);
#5456=VERTEX_POINT('',#19345);
#5457=VERTEX_POINT('',#19349);
#5458=VERTEX_POINT('',#19353);
#5459=VERTEX_POINT('',#19357);
#5460=VERTEX_POINT('',#19361);
#5461=VERTEX_POINT('',#19362);
#5462=VERTEX_POINT('',#19364);
#5463=VERTEX_POINT('',#19366);
#5464=VERTEX_POINT('',#19370);
#5465=VERTEX_POINT('',#19372);
#5466=VERTEX_POINT('',#19376);
#5467=VERTEX_POINT('',#19378);
#5468=VERTEX_POINT('',#19382);
#5469=VERTEX_POINT('',#19384);
#5470=VERTEX_POINT('',#19388);
#5471=VERTEX_POINT('',#19390);
#5472=VERTEX_POINT('',#19394);
#5473=VERTEX_POINT('',#19396);
#5474=VERTEX_POINT('',#19400);
#5475=VERTEX_POINT('',#19402);
#5476=VERTEX_POINT('',#19406);
#5477=VERTEX_POINT('',#19408);
#5478=VERTEX_POINT('',#19412);
#5479=VERTEX_POINT('',#19414);
#5480=VERTEX_POINT('',#19418);
#5481=VERTEX_POINT('',#19420);
#5482=VERTEX_POINT('',#19424);
#5483=VERTEX_POINT('',#19426);
#5484=VERTEX_POINT('',#19437);
#5485=VERTEX_POINT('',#19438);
#5486=VERTEX_POINT('',#19441);
#5487=VERTEX_POINT('',#19443);
#5488=VERTEX_POINT('',#19447);
#5489=VERTEX_POINT('',#19451);
#5490=VERTEX_POINT('',#19453);
#5491=VERTEX_POINT('',#19457);
#5492=VERTEX_POINT('',#19462);
#5493=VERTEX_POINT('',#19466);
#5494=VERTEX_POINT('',#19472);
#5495=VERTEX_POINT('',#19473);
#5496=VERTEX_POINT('',#19476);
#5497=VERTEX_POINT('',#19478);
#5498=VERTEX_POINT('',#19482);
#5499=VERTEX_POINT('',#19486);
#5500=VERTEX_POINT('',#19488);
#5501=VERTEX_POINT('',#19491);
#5502=VERTEX_POINT('',#19495);
#5503=VERTEX_POINT('',#19499);
#5504=VERTEX_POINT('',#19507);
#5505=VERTEX_POINT('',#19508);
#5506=VERTEX_POINT('',#19511);
#5507=VERTEX_POINT('',#19512);
#5508=VERTEX_POINT('',#19515);
#5509=VERTEX_POINT('',#19516);
#5510=VERTEX_POINT('',#19519);
#5511=VERTEX_POINT('',#19520);
#5512=VERTEX_POINT('',#19523);
#5513=VERTEX_POINT('',#19524);
#5514=VERTEX_POINT('',#19527);
#5515=VERTEX_POINT('',#19528);
#5516=VERTEX_POINT('',#19531);
#5517=VERTEX_POINT('',#19532);
#5518=VERTEX_POINT('',#19535);
#5519=VERTEX_POINT('',#19536);
#5520=VERTEX_POINT('',#19540);
#5521=VERTEX_POINT('',#19541);
#5522=VERTEX_POINT('',#19564);
#5523=VERTEX_POINT('',#19566);
#5524=VERTEX_POINT('',#19591);
#5525=VERTEX_POINT('',#19593);
#5526=VERTEX_POINT('',#19616);
#5527=VERTEX_POINT('',#19618);
#5528=VERTEX_POINT('',#19641);
#5529=VERTEX_POINT('',#19643);
#5530=VERTEX_POINT('',#19656);
#5531=VERTEX_POINT('',#19659);
#5532=VERTEX_POINT('',#19672);
#5533=VERTEX_POINT('',#19674);
#5534=VERTEX_POINT('',#19697);
#5535=VERTEX_POINT('',#19699);
#5536=VERTEX_POINT('',#19722);
#5537=VERTEX_POINT('',#19724);
#5538=VERTEX_POINT('',#19747);
#5539=VERTEX_POINT('',#19749);
#5540=VERTEX_POINT('',#19774);
#5541=VERTEX_POINT('',#19778);
#5542=VERTEX_POINT('',#19803);
#5543=VERTEX_POINT('',#19807);
#5544=VERTEX_POINT('',#19832);
#5545=VERTEX_POINT('',#19836);
#5546=VERTEX_POINT('',#19837);
#5547=VERTEX_POINT('',#19864);
#5548=VERTEX_POINT('',#19868);
#5549=VERTEX_POINT('',#19893);
#5550=VERTEX_POINT('',#19897);
#5551=VERTEX_POINT('',#19922);
#5552=VERTEX_POINT('',#19926);
#5553=VERTEX_POINT('',#19951);
#5554=VERTEX_POINT('',#19954);
#5555=VERTEX_POINT('',#19956);
#5556=VERTEX_POINT('',#19988);
#5557=VERTEX_POINT('',#19990);
#5558=VERTEX_POINT('',#19993);
#5559=VERTEX_POINT('',#19997);
#5560=VERTEX_POINT('',#20002);
#5561=VERTEX_POINT('',#20004);
#5562=VERTEX_POINT('',#20007);
#5563=VERTEX_POINT('',#20011);
#5564=VERTEX_POINT('',#20023);
#5565=VERTEX_POINT('',#20025);
#5566=VERTEX_POINT('',#20029);
#5567=VERTEX_POINT('',#20031);
#5568=VERTEX_POINT('',#20035);
#5569=VERTEX_POINT('',#20037);
#5570=VERTEX_POINT('',#20041);
#5571=VERTEX_POINT('',#20043);
#5572=VERTEX_POINT('',#20047);
#5573=VERTEX_POINT('',#20049);
#5574=VERTEX_POINT('',#20053);
#5575=VERTEX_POINT('',#20055);
#5576=VERTEX_POINT('',#20059);
#5577=VERTEX_POINT('',#20061);
#5578=VERTEX_POINT('',#20065);
#5579=VERTEX_POINT('',#20067);
#5580=VERTEX_POINT('',#20071);
#5581=VERTEX_POINT('',#20073);
#5582=VERTEX_POINT('',#20077);
#5583=VERTEX_POINT('',#20079);
#5584=VERTEX_POINT('',#20083);
#5585=VERTEX_POINT('',#20084);
#5586=VERTEX_POINT('',#20086);
#5587=VERTEX_POINT('',#20088);
#5588=VERTEX_POINT('',#20092);
#5589=VERTEX_POINT('',#20094);
#5590=VERTEX_POINT('',#20098);
#5591=VERTEX_POINT('',#20100);
#5592=VERTEX_POINT('',#20110);
#5593=VERTEX_POINT('',#20112);
#5594=VERTEX_POINT('',#20116);
#5595=VERTEX_POINT('',#20118);
#5596=VERTEX_POINT('',#20122);
#5597=VERTEX_POINT('',#20124);
#5598=VERTEX_POINT('',#20128);
#5599=VERTEX_POINT('',#20130);
#5600=VERTEX_POINT('',#20134);
#5601=VERTEX_POINT('',#20136);
#5602=VERTEX_POINT('',#20140);
#5603=VERTEX_POINT('',#20141);
#5604=VERTEX_POINT('',#20145);
#5605=VERTEX_POINT('',#20147);
#5606=VERTEX_POINT('',#20151);
#5607=VERTEX_POINT('',#20152);
#5608=VERTEX_POINT('',#20156);
#5609=VERTEX_POINT('',#20158);
#5610=VERTEX_POINT('',#20162);
#5611=VERTEX_POINT('',#20163);
#5612=VERTEX_POINT('',#20167);
#5613=VERTEX_POINT('',#20169);
#5614=VERTEX_POINT('',#20173);
#5615=VERTEX_POINT('',#20174);
#5616=VERTEX_POINT('',#20178);
#5617=VERTEX_POINT('',#20180);
#5618=VERTEX_POINT('',#20184);
#5619=VERTEX_POINT('',#20186);
#5620=VERTEX_POINT('',#20188);
#5621=VERTEX_POINT('',#20190);
#5622=VERTEX_POINT('',#20192);
#5623=VERTEX_POINT('',#20194);
#5624=VERTEX_POINT('',#20196);
#5625=VERTEX_POINT('',#20198);
#5626=VERTEX_POINT('',#20203);
#5627=VERTEX_POINT('',#20205);
#5628=VERTEX_POINT('',#20207);
#5629=VERTEX_POINT('',#20209);
#5630=VERTEX_POINT('',#20211);
#5631=VERTEX_POINT('',#20213);
#5632=VERTEX_POINT('',#20215);
#5633=VERTEX_POINT('',#20217);
#5634=VERTEX_POINT('',#20222);
#5635=VERTEX_POINT('',#20224);
#5636=VERTEX_POINT('',#20228);
#5637=VERTEX_POINT('',#20230);
#5638=VERTEX_POINT('',#20234);
#5639=VERTEX_POINT('',#20236);
#5640=VERTEX_POINT('',#20240);
#5641=VERTEX_POINT('',#20242);
#5642=VERTEX_POINT('',#20263);
#5643=VERTEX_POINT('',#20265);
#5644=VERTEX_POINT('',#20269);
#5645=VERTEX_POINT('',#20271);
#5646=VERTEX_POINT('',#20278);
#5647=VERTEX_POINT('',#20279);
#5648=VERTEX_POINT('',#20281);
#5649=VERTEX_POINT('',#20283);
#5650=VERTEX_POINT('',#20287);
#5651=VERTEX_POINT('',#20288);
#5652=VERTEX_POINT('',#20290);
#5653=VERTEX_POINT('',#20292);
#5654=VERTEX_POINT('',#20296);
#5655=VERTEX_POINT('',#20297);
#5656=VERTEX_POINT('',#20299);
#5657=VERTEX_POINT('',#20301);
#5658=VERTEX_POINT('',#20305);
#5659=VERTEX_POINT('',#20306);
#5660=VERTEX_POINT('',#20308);
#5661=VERTEX_POINT('',#20310);
#5662=VERTEX_POINT('',#20318);
#5663=VERTEX_POINT('',#20329);
#5664=VERTEX_POINT('',#20331);
#5665=VERTEX_POINT('',#20335);
#5666=VERTEX_POINT('',#20342);
#5667=VERTEX_POINT('',#20343);
#5668=VERTEX_POINT('',#20345);
#5669=VERTEX_POINT('',#20347);
#5670=VERTEX_POINT('',#20351);
#5671=VERTEX_POINT('',#20352);
#5672=VERTEX_POINT('',#20354);
#5673=VERTEX_POINT('',#20356);
#5674=VERTEX_POINT('',#20360);
#5675=VERTEX_POINT('',#20361);
#5676=VERTEX_POINT('',#20363);
#5677=VERTEX_POINT('',#20365);
#5678=VERTEX_POINT('',#20369);
#5679=VERTEX_POINT('',#20370);
#5680=VERTEX_POINT('',#20372);
#5681=VERTEX_POINT('',#20374);
#5682=VERTEX_POINT('',#20382);
#5683=VERTEX_POINT('',#20393);
#5684=VERTEX_POINT('',#20397);
#5685=VERTEX_POINT('',#20400);
#5686=VERTEX_POINT('',#20406);
#5687=VERTEX_POINT('',#20408);
#5688=VERTEX_POINT('',#20413);
#5689=VERTEX_POINT('',#20415);
#5690=VERTEX_POINT('',#20420);
#5691=VERTEX_POINT('',#20422);
#5692=VERTEX_POINT('',#20426);
#5693=VERTEX_POINT('',#20427);
#5694=VERTEX_POINT('',#20429);
#5695=VERTEX_POINT('',#20431);
#5696=VERTEX_POINT('',#20435);
#5697=VERTEX_POINT('',#20437);
#5698=VERTEX_POINT('',#20441);
#5699=VERTEX_POINT('',#20443);
#5700=VERTEX_POINT('',#20453);
#5701=VERTEX_POINT('',#20456);
#5702=VERTEX_POINT('',#20462);
#5703=VERTEX_POINT('',#20463);
#5704=VERTEX_POINT('',#20467);
#5705=VERTEX_POINT('',#20468);
#5706=VERTEX_POINT('',#20475);
#5707=VERTEX_POINT('',#20477);
#5708=VERTEX_POINT('',#20496);
#5709=VERTEX_POINT('',#20502);
#5710=VERTEX_POINT('',#20505);
#5711=VERTEX_POINT('',#20509);
#5712=VERTEX_POINT('',#20510);
#5713=VERTEX_POINT('',#20512);
#5714=VERTEX_POINT('',#20514);
#5715=VERTEX_POINT('',#20518);
#5716=VERTEX_POINT('',#20520);
#5717=VERTEX_POINT('',#20524);
#5718=VERTEX_POINT('',#20526);
#5719=VERTEX_POINT('',#20537);
#5720=VERTEX_POINT('',#20538);
#5721=VERTEX_POINT('',#20542);
#5722=VERTEX_POINT('',#20544);
#5723=VERTEX_POINT('',#20546);
#5724=VERTEX_POINT('',#20549);
#5725=VERTEX_POINT('',#20553);
#5726=VERTEX_POINT('',#20554);
#5727=VERTEX_POINT('',#20558);
#5728=VERTEX_POINT('',#20560);
#5729=VERTEX_POINT('',#20562);
#5730=VERTEX_POINT('',#20565);
#5731=VERTEX_POINT('',#20569);
#5732=VERTEX_POINT('',#20570);
#5733=VERTEX_POINT('',#20574);
#5734=VERTEX_POINT('',#20576);
#5735=VERTEX_POINT('',#20578);
#5736=VERTEX_POINT('',#20581);
#5737=VERTEX_POINT('',#20585);
#5738=VERTEX_POINT('',#20586);
#5739=VERTEX_POINT('',#20590);
#5740=VERTEX_POINT('',#20592);
#5741=VERTEX_POINT('',#20594);
#5742=VERTEX_POINT('',#20597);
#5743=VERTEX_POINT('',#20602);
#5744=VERTEX_POINT('',#20604);
#5745=VERTEX_POINT('',#20606);
#5746=VERTEX_POINT('',#20608);
#5747=VERTEX_POINT('',#20613);
#5748=VERTEX_POINT('',#20615);
#5749=VERTEX_POINT('',#20617);
#5750=VERTEX_POINT('',#20619);
#5751=VERTEX_POINT('',#20623);
#5752=VERTEX_POINT('',#20625);
#5753=VERTEX_POINT('',#20627);
#5754=VERTEX_POINT('',#20629);
#5755=VERTEX_POINT('',#20632);
#5756=VERTEX_POINT('',#20634);
#5757=VERTEX_POINT('',#20636);
#5758=VERTEX_POINT('',#20638);
#5759=VERTEX_POINT('',#20642);
#5760=VERTEX_POINT('',#20646);
#5761=VERTEX_POINT('',#20650);
#5762=VERTEX_POINT('',#20654);
#5763=VERTEX_POINT('',#20660);
#5764=VERTEX_POINT('',#20664);
#5765=VERTEX_POINT('',#20668);
#5766=VERTEX_POINT('',#20672);
#5767=VERTEX_POINT('',#20680);
#5768=VERTEX_POINT('',#20681);
#5769=VERTEX_POINT('',#20683);
#5770=VERTEX_POINT('',#20685);
#5771=VERTEX_POINT('',#20689);
#5772=VERTEX_POINT('',#20691);
#5773=VERTEX_POINT('',#20695);
#5774=VERTEX_POINT('',#20697);
#5775=VERTEX_POINT('',#20701);
#5776=VERTEX_POINT('',#20703);
#5777=VERTEX_POINT('',#20707);
#5778=VERTEX_POINT('',#20709);
#5779=VERTEX_POINT('',#20713);
#5780=VERTEX_POINT('',#20715);
#5781=VERTEX_POINT('',#20719);
#5782=VERTEX_POINT('',#20721);
#5783=VERTEX_POINT('',#20731);
#5784=VERTEX_POINT('',#20732);
#5785=VERTEX_POINT('',#20734);
#5786=VERTEX_POINT('',#20736);
#5787=VERTEX_POINT('',#20740);
#5788=VERTEX_POINT('',#20742);
#5789=VERTEX_POINT('',#20746);
#5790=VERTEX_POINT('',#20748);
#5791=VERTEX_POINT('',#20752);
#5792=VERTEX_POINT('',#20754);
#5793=VERTEX_POINT('',#20758);
#5794=VERTEX_POINT('',#20760);
#5795=VERTEX_POINT('',#20764);
#5796=VERTEX_POINT('',#20766);
#5797=VERTEX_POINT('',#20770);
#5798=VERTEX_POINT('',#20772);
#5799=VERTEX_POINT('',#20785);
#5800=VERTEX_POINT('',#20786);
#5801=VERTEX_POINT('',#20788);
#5802=VERTEX_POINT('',#20790);
#5803=VERTEX_POINT('',#20794);
#5804=VERTEX_POINT('',#20796);
#5805=VERTEX_POINT('',#20800);
#5806=VERTEX_POINT('',#20802);
#5807=VERTEX_POINT('',#20806);
#5808=VERTEX_POINT('',#20808);
#5809=VERTEX_POINT('',#20812);
#5810=VERTEX_POINT('',#20814);
#5811=VERTEX_POINT('',#20823);
#5812=VERTEX_POINT('',#20826);
#5813=VERTEX_POINT('',#20829);
#5814=VERTEX_POINT('',#20833);
#5815=VERTEX_POINT('',#20837);
#5816=VERTEX_POINT('',#20841);
#5817=VERTEX_POINT('',#20844);
#5818=VERTEX_POINT('',#20852);
#5819=VERTEX_POINT('',#20853);
#5820=VERTEX_POINT('',#20856);
#5821=VERTEX_POINT('',#20858);
#5822=VERTEX_POINT('',#20862);
#5823=VERTEX_POINT('',#20866);
#5824=VERTEX_POINT('',#20868);
#5825=VERTEX_POINT('',#20872);
#5826=VERTEX_POINT('',#20877);
#5827=VERTEX_POINT('',#20881);
#5828=VERTEX_POINT('',#20887);
#5829=VERTEX_POINT('',#20888);
#5830=VERTEX_POINT('',#20891);
#5831=VERTEX_POINT('',#20893);
#5832=VERTEX_POINT('',#20897);
#5833=VERTEX_POINT('',#20901);
#5834=VERTEX_POINT('',#20903);
#5835=VERTEX_POINT('',#20906);
#5836=VERTEX_POINT('',#20910);
#5837=VERTEX_POINT('',#20914);
#5838=VERTEX_POINT('',#20922);
#5839=VERTEX_POINT('',#20923);
#5840=VERTEX_POINT('',#20926);
#5841=VERTEX_POINT('',#20927);
#5842=VERTEX_POINT('',#20930);
#5843=VERTEX_POINT('',#20931);
#5844=VERTEX_POINT('',#20934);
#5845=VERTEX_POINT('',#20935);
#5846=VERTEX_POINT('',#20938);
#5847=VERTEX_POINT('',#20939);
#5848=VERTEX_POINT('',#20942);
#5849=VERTEX_POINT('',#20943);
#5850=VERTEX_POINT('',#20946);
#5851=VERTEX_POINT('',#20947);
#5852=VERTEX_POINT('',#20951);
#5853=VERTEX_POINT('',#20952);
#5854=VERTEX_POINT('',#20975);
#5855=VERTEX_POINT('',#20977);
#5856=VERTEX_POINT('',#21002);
#5857=VERTEX_POINT('',#21004);
#5858=VERTEX_POINT('',#21027);
#5859=VERTEX_POINT('',#21029);
#5860=VERTEX_POINT('',#21052);
#5861=VERTEX_POINT('',#21054);
#5862=VERTEX_POINT('',#21057);
#5863=VERTEX_POINT('',#21059);
#5864=VERTEX_POINT('',#21082);
#5865=VERTEX_POINT('',#21084);
#5866=VERTEX_POINT('',#21107);
#5867=VERTEX_POINT('',#21109);
#5868=VERTEX_POINT('',#21132);
#5869=VERTEX_POINT('',#21134);
#5870=VERTEX_POINT('',#21159);
#5871=VERTEX_POINT('',#21163);
#5872=VERTEX_POINT('',#21188);
#5873=VERTEX_POINT('',#21192);
#5874=VERTEX_POINT('',#21217);
#5875=VERTEX_POINT('',#21219);
#5876=VERTEX_POINT('',#21223);
#5877=VERTEX_POINT('',#21248);
#5878=VERTEX_POINT('',#21252);
#5879=VERTEX_POINT('',#21277);
#5880=VERTEX_POINT('',#21281);
#5881=VERTEX_POINT('',#21306);
#5882=VERTEX_POINT('',#21309);
#5883=VERTEX_POINT('',#21311);
#5884=VERTEX_POINT('',#21343);
#5885=VERTEX_POINT('',#21345);
#5886=VERTEX_POINT('',#21348);
#5887=VERTEX_POINT('',#21352);
#5888=VERTEX_POINT('',#21357);
#5889=VERTEX_POINT('',#21359);
#5890=VERTEX_POINT('',#21362);
#5891=VERTEX_POINT('',#21366);
#5892=VERTEX_POINT('',#21377);
#5893=VERTEX_POINT('',#21378);
#5894=VERTEX_POINT('',#21380);
#5895=VERTEX_POINT('',#21382);
#5896=VERTEX_POINT('',#21386);
#5897=VERTEX_POINT('',#21388);
#5898=VERTEX_POINT('',#21392);
#5899=VERTEX_POINT('',#21394);
#5900=VERTEX_POINT('',#21398);
#5901=VERTEX_POINT('',#21400);
#5902=VERTEX_POINT('',#21404);
#5903=VERTEX_POINT('',#21406);
#5904=VERTEX_POINT('',#21415);
#5905=VERTEX_POINT('',#21418);
#5906=VERTEX_POINT('',#21421);
#5907=VERTEX_POINT('',#21425);
#5908=VERTEX_POINT('',#21429);
#5909=VERTEX_POINT('',#21433);
#5910=VERTEX_POINT('',#21436);
#5911=VERTEX_POINT('',#21444);
#5912=VERTEX_POINT('',#21446);
#5913=VERTEX_POINT('',#21451);
#5914=VERTEX_POINT('',#21453);
#5915=VERTEX_POINT('',#21456);
#5916=VERTEX_POINT('',#21458);
#5917=VERTEX_POINT('',#21463);
#5918=VERTEX_POINT('',#21467);
#5919=VERTEX_POINT('',#21469);
#5920=VERTEX_POINT('',#21474);
#5921=VERTEX_POINT('',#21481);
#5922=VERTEX_POINT('',#21483);
#5923=VERTEX_POINT('',#21487);
#5924=VERTEX_POINT('',#21490);
#5925=VERTEX_POINT('',#21494);
#5926=VERTEX_POINT('',#21496);
#5927=VERTEX_POINT('',#21503);
#5928=VERTEX_POINT('',#21505);
#5929=VERTEX_POINT('',#21509);
#5930=VERTEX_POINT('',#21511);
#5931=VERTEX_POINT('',#21518);
#5932=VERTEX_POINT('',#21520);
#5933=VERTEX_POINT('',#21527);
#5934=VERTEX_POINT('',#21529);
#5935=VERTEX_POINT('',#21536);
#5936=VERTEX_POINT('',#21538);
#5937=VERTEX_POINT('',#21542);
#5938=VERTEX_POINT('',#21544);
#5939=VERTEX_POINT('',#21551);
#5940=VERTEX_POINT('',#21552);
#5941=VERTEX_POINT('',#21563);
#5942=VERTEX_POINT('',#21592);
#5943=VERTEX_POINT('',#21594);
#5944=VERTEX_POINT('',#21605);
#5945=VERTEX_POINT('',#21616);
#5946=VERTEX_POINT('',#21638);
#5947=VERTEX_POINT('',#21639);
#5948=VERTEX_POINT('',#21676);
#5949=VERTEX_POINT('',#21678);
#5950=VERTEX_POINT('',#21689);
#5951=VERTEX_POINT('',#21719);
#5952=VERTEX_POINT('',#21722);
#5953=VERTEX_POINT('',#21725);
#5954=VERTEX_POINT('',#21726);
#5955=VERTEX_POINT('',#21745);
#5956=VERTEX_POINT('',#21766);
#5957=VERTEX_POINT('',#21767);
#5958=VERTEX_POINT('',#21786);
#5959=VERTEX_POINT('',#21808);
#5960=VERTEX_POINT('',#21810);
#5961=VERTEX_POINT('',#21848);
#5962=VERTEX_POINT('',#21849);
#5963=VERTEX_POINT('',#21888);
#5964=VERTEX_POINT('',#21891);
#5965=VERTEX_POINT('',#21896);
#5966=VERTEX_POINT('',#21898);
#5967=VERTEX_POINT('',#21899);
#5968=VERTEX_POINT('',#21901);
#5969=VERTEX_POINT('',#21903);
#5970=VERTEX_POINT('',#21905);
#5971=VERTEX_POINT('',#21907);
#5972=VERTEX_POINT('',#21909);
#5973=VERTEX_POINT('',#21911);
#5974=VERTEX_POINT('',#21913);
#5975=VERTEX_POINT('',#21915);
#5976=VERTEX_POINT('',#21917);
#5977=VERTEX_POINT('',#21919);
#5978=VERTEX_POINT('',#21921);
#5979=VERTEX_POINT('',#21923);
#5980=VERTEX_POINT('',#21925);
#5981=VERTEX_POINT('',#21927);
#5982=VERTEX_POINT('',#21929);
#5983=VERTEX_POINT('',#21931);
#5984=VERTEX_POINT('',#21933);
#5985=VERTEX_POINT('',#21935);
#5986=VERTEX_POINT('',#21937);
#5987=VERTEX_POINT('',#21939);
#5988=VERTEX_POINT('',#21941);
#5989=VERTEX_POINT('',#21943);
#5990=VERTEX_POINT('',#21945);
#5991=VERTEX_POINT('',#21947);
#5992=VERTEX_POINT('',#21949);
#5993=VERTEX_POINT('',#21951);
#5994=VERTEX_POINT('',#21953);
#5995=VERTEX_POINT('',#21955);
#5996=VERTEX_POINT('',#21957);
#5997=VERTEX_POINT('',#21959);
#5998=VERTEX_POINT('',#21961);
#5999=VERTEX_POINT('',#21963);
#6000=VERTEX_POINT('',#21965);
#6001=VERTEX_POINT('',#21967);
#6002=VERTEX_POINT('',#21969);
#6003=VERTEX_POINT('',#21971);
#6004=VERTEX_POINT('',#21973);
#6005=VERTEX_POINT('',#21975);
#6006=VERTEX_POINT('',#21979);
#6007=VERTEX_POINT('',#21984);
#6008=VERTEX_POINT('',#21986);
#6009=VERTEX_POINT('',#21987);
#6010=VERTEX_POINT('',#21989);
#6011=VERTEX_POINT('',#21991);
#6012=VERTEX_POINT('',#21993);
#6013=VERTEX_POINT('',#21995);
#6014=VERTEX_POINT('',#21997);
#6015=VERTEX_POINT('',#21999);
#6016=VERTEX_POINT('',#22001);
#6017=VERTEX_POINT('',#22003);
#6018=VERTEX_POINT('',#22005);
#6019=VERTEX_POINT('',#22007);
#6020=VERTEX_POINT('',#22009);
#6021=VERTEX_POINT('',#22011);
#6022=VERTEX_POINT('',#22013);
#6023=VERTEX_POINT('',#22015);
#6024=VERTEX_POINT('',#22017);
#6025=VERTEX_POINT('',#22019);
#6026=VERTEX_POINT('',#22021);
#6027=VERTEX_POINT('',#22023);
#6028=VERTEX_POINT('',#22025);
#6029=VERTEX_POINT('',#22027);
#6030=VERTEX_POINT('',#22029);
#6031=VERTEX_POINT('',#22031);
#6032=VERTEX_POINT('',#22033);
#6033=VERTEX_POINT('',#22035);
#6034=VERTEX_POINT('',#22037);
#6035=VERTEX_POINT('',#22039);
#6036=VERTEX_POINT('',#22041);
#6037=VERTEX_POINT('',#22043);
#6038=VERTEX_POINT('',#22045);
#6039=VERTEX_POINT('',#22047);
#6040=VERTEX_POINT('',#22049);
#6041=VERTEX_POINT('',#22051);
#6042=VERTEX_POINT('',#22053);
#6043=VERTEX_POINT('',#22055);
#6044=VERTEX_POINT('',#22057);
#6045=VERTEX_POINT('',#22059);
#6046=VERTEX_POINT('',#22061);
#6047=VERTEX_POINT('',#22063);
#6048=VERTEX_POINT('',#22067);
#6049=VERTEX_POINT('',#22154);
#6050=VERTEX_POINT('',#22156);
#6051=VERTEX_POINT('',#22161);
#6052=VERTEX_POINT('',#22163);
#6053=VERTEX_POINT('',#22166);
#6054=VERTEX_POINT('',#22168);
#6055=VERTEX_POINT('',#22173);
#6056=VERTEX_POINT('',#22178);
#6057=VERTEX_POINT('',#22184);
#6058=VERTEX_POINT('',#22186);
#6059=VERTEX_POINT('',#22190);
#6060=VERTEX_POINT('',#22192);
#6061=VERTEX_POINT('',#22199);
#6062=VERTEX_POINT('',#22201);
#6063=VERTEX_POINT('',#22205);
#6064=VERTEX_POINT('',#22207);
#6065=VERTEX_POINT('',#22214);
#6066=VERTEX_POINT('',#22216);
#6067=VERTEX_POINT('',#22223);
#6068=VERTEX_POINT('',#22225);
#6069=VERTEX_POINT('',#22232);
#6070=VERTEX_POINT('',#22234);
#6071=VERTEX_POINT('',#22238);
#6072=VERTEX_POINT('',#22240);
#6073=VERTEX_POINT('',#22247);
#6074=VERTEX_POINT('',#22248);
#6075=VERTEX_POINT('',#22259);
#6076=VERTEX_POINT('',#22288);
#6077=VERTEX_POINT('',#22290);
#6078=VERTEX_POINT('',#22301);
#6079=VERTEX_POINT('',#22312);
#6080=VERTEX_POINT('',#22334);
#6081=VERTEX_POINT('',#22335);
#6082=VERTEX_POINT('',#22372);
#6083=VERTEX_POINT('',#22374);
#6084=VERTEX_POINT('',#22385);
#6085=VERTEX_POINT('',#22415);
#6086=VERTEX_POINT('',#22418);
#6087=VERTEX_POINT('',#22421);
#6088=VERTEX_POINT('',#22422);
#6089=VERTEX_POINT('',#22441);
#6090=VERTEX_POINT('',#22462);
#6091=VERTEX_POINT('',#22463);
#6092=VERTEX_POINT('',#22482);
#6093=VERTEX_POINT('',#22504);
#6094=VERTEX_POINT('',#22506);
#6095=VERTEX_POINT('',#22544);
#6096=VERTEX_POINT('',#22545);
#6097=VERTEX_POINT('',#22584);
#6098=VERTEX_POINT('',#22587);
#6099=VERTEX_POINT('',#22592);
#6100=VERTEX_POINT('',#22594);
#6101=VERTEX_POINT('',#22595);
#6102=VERTEX_POINT('',#22597);
#6103=VERTEX_POINT('',#22599);
#6104=VERTEX_POINT('',#22601);
#6105=VERTEX_POINT('',#22603);
#6106=VERTEX_POINT('',#22605);
#6107=VERTEX_POINT('',#22607);
#6108=VERTEX_POINT('',#22609);
#6109=VERTEX_POINT('',#22611);
#6110=VERTEX_POINT('',#22613);
#6111=VERTEX_POINT('',#22615);
#6112=VERTEX_POINT('',#22617);
#6113=VERTEX_POINT('',#22619);
#6114=VERTEX_POINT('',#22621);
#6115=VERTEX_POINT('',#22623);
#6116=VERTEX_POINT('',#22625);
#6117=VERTEX_POINT('',#22627);
#6118=VERTEX_POINT('',#22629);
#6119=VERTEX_POINT('',#22631);
#6120=VERTEX_POINT('',#22633);
#6121=VERTEX_POINT('',#22635);
#6122=VERTEX_POINT('',#22637);
#6123=VERTEX_POINT('',#22639);
#6124=VERTEX_POINT('',#22641);
#6125=VERTEX_POINT('',#22643);
#6126=VERTEX_POINT('',#22645);
#6127=VERTEX_POINT('',#22647);
#6128=VERTEX_POINT('',#22649);
#6129=VERTEX_POINT('',#22651);
#6130=VERTEX_POINT('',#22653);
#6131=VERTEX_POINT('',#22655);
#6132=VERTEX_POINT('',#22657);
#6133=VERTEX_POINT('',#22659);
#6134=VERTEX_POINT('',#22661);
#6135=VERTEX_POINT('',#22663);
#6136=VERTEX_POINT('',#22665);
#6137=VERTEX_POINT('',#22667);
#6138=VERTEX_POINT('',#22669);
#6139=VERTEX_POINT('',#22671);
#6140=VERTEX_POINT('',#22673);
#6141=VERTEX_POINT('',#22675);
#6142=VERTEX_POINT('',#22677);
#6143=VERTEX_POINT('',#22679);
#6144=VERTEX_POINT('',#22681);
#6145=VERTEX_POINT('',#22683);
#6146=VERTEX_POINT('',#22685);
#6147=VERTEX_POINT('',#22687);
#6148=VERTEX_POINT('',#22689);
#6149=VERTEX_POINT('',#22691);
#6150=VERTEX_POINT('',#22693);
#6151=VERTEX_POINT('',#22695);
#6152=VERTEX_POINT('',#22697);
#6153=VERTEX_POINT('',#22699);
#6154=VERTEX_POINT('',#22701);
#6155=VERTEX_POINT('',#22703);
#6156=VERTEX_POINT('',#22705);
#6157=VERTEX_POINT('',#22707);
#6158=VERTEX_POINT('',#22709);
#6159=VERTEX_POINT('',#22711);
#6160=VERTEX_POINT('',#22713);
#6161=VERTEX_POINT('',#22715);
#6162=VERTEX_POINT('',#22717);
#6163=VERTEX_POINT('',#22719);
#6164=VERTEX_POINT('',#22721);
#6165=VERTEX_POINT('',#22723);
#6166=VERTEX_POINT('',#22725);
#6167=VERTEX_POINT('',#22727);
#6168=VERTEX_POINT('',#22729);
#6169=VERTEX_POINT('',#22731);
#6170=VERTEX_POINT('',#22733);
#6171=VERTEX_POINT('',#22735);
#6172=VERTEX_POINT('',#22737);
#6173=VERTEX_POINT('',#22739);
#6174=VERTEX_POINT('',#22741);
#6175=VERTEX_POINT('',#22743);
#6176=VERTEX_POINT('',#22745);
#6177=VERTEX_POINT('',#22747);
#6178=VERTEX_POINT('',#22749);
#6179=VERTEX_POINT('',#22751);
#6180=VERTEX_POINT('',#22755);
#6181=VERTEX_POINT('',#22760);
#6182=VERTEX_POINT('',#22762);
#6183=VERTEX_POINT('',#22763);
#6184=VERTEX_POINT('',#22765);
#6185=VERTEX_POINT('',#22767);
#6186=VERTEX_POINT('',#22769);
#6187=VERTEX_POINT('',#22771);
#6188=VERTEX_POINT('',#22773);
#6189=VERTEX_POINT('',#22775);
#6190=VERTEX_POINT('',#22777);
#6191=VERTEX_POINT('',#22779);
#6192=VERTEX_POINT('',#22781);
#6193=VERTEX_POINT('',#22783);
#6194=VERTEX_POINT('',#22785);
#6195=VERTEX_POINT('',#22787);
#6196=VERTEX_POINT('',#22789);
#6197=VERTEX_POINT('',#22791);
#6198=VERTEX_POINT('',#22793);
#6199=VERTEX_POINT('',#22795);
#6200=VERTEX_POINT('',#22797);
#6201=VERTEX_POINT('',#22799);
#6202=VERTEX_POINT('',#22801);
#6203=VERTEX_POINT('',#22803);
#6204=VERTEX_POINT('',#22805);
#6205=VERTEX_POINT('',#22807);
#6206=VERTEX_POINT('',#22809);
#6207=VERTEX_POINT('',#22811);
#6208=VERTEX_POINT('',#22813);
#6209=VERTEX_POINT('',#22815);
#6210=VERTEX_POINT('',#22817);
#6211=VERTEX_POINT('',#22819);
#6212=VERTEX_POINT('',#22821);
#6213=VERTEX_POINT('',#22823);
#6214=VERTEX_POINT('',#22825);
#6215=VERTEX_POINT('',#22827);
#6216=VERTEX_POINT('',#22829);
#6217=VERTEX_POINT('',#22831);
#6218=VERTEX_POINT('',#22833);
#6219=VERTEX_POINT('',#22835);
#6220=VERTEX_POINT('',#22837);
#6221=VERTEX_POINT('',#22839);
#6222=VERTEX_POINT('',#22841);
#6223=VERTEX_POINT('',#22843);
#6224=VERTEX_POINT('',#22845);
#6225=VERTEX_POINT('',#22847);
#6226=VERTEX_POINT('',#22849);
#6227=VERTEX_POINT('',#22851);
#6228=VERTEX_POINT('',#22853);
#6229=VERTEX_POINT('',#22855);
#6230=VERTEX_POINT('',#22857);
#6231=VERTEX_POINT('',#22859);
#6232=VERTEX_POINT('',#22861);
#6233=VERTEX_POINT('',#22863);
#6234=VERTEX_POINT('',#22865);
#6235=VERTEX_POINT('',#22867);
#6236=VERTEX_POINT('',#22869);
#6237=VERTEX_POINT('',#22871);
#6238=VERTEX_POINT('',#22873);
#6239=VERTEX_POINT('',#22875);
#6240=VERTEX_POINT('',#22877);
#6241=VERTEX_POINT('',#22879);
#6242=VERTEX_POINT('',#22881);
#6243=VERTEX_POINT('',#22883);
#6244=VERTEX_POINT('',#22885);
#6245=VERTEX_POINT('',#22887);
#6246=VERTEX_POINT('',#22889);
#6247=VERTEX_POINT('',#22891);
#6248=VERTEX_POINT('',#22893);
#6249=VERTEX_POINT('',#22895);
#6250=VERTEX_POINT('',#22897);
#6251=VERTEX_POINT('',#22899);
#6252=VERTEX_POINT('',#22901);
#6253=VERTEX_POINT('',#22903);
#6254=VERTEX_POINT('',#22905);
#6255=VERTEX_POINT('',#22907);
#6256=VERTEX_POINT('',#22909);
#6257=VERTEX_POINT('',#22911);
#6258=VERTEX_POINT('',#22913);
#6259=VERTEX_POINT('',#22915);
#6260=VERTEX_POINT('',#22917);
#6261=VERTEX_POINT('',#22919);
#6262=VERTEX_POINT('',#22923);
#6263=VERTEX_POINT('',#23089);
#6264=VERTEX_POINT('',#23092);
#6265=VERTEX_POINT('',#23096);
#6266=VERTEX_POINT('',#23100);
#6267=VERTEX_POINT('',#23104);
#6268=VERTEX_POINT('',#23107);
#6269=VERTEX_POINT('',#23111);
#6270=VERTEX_POINT('',#23115);
#6271=VERTEX_POINT('',#23120);
#6272=VERTEX_POINT('',#23121);
#6273=VERTEX_POINT('',#23123);
#6274=VERTEX_POINT('',#23125);
#6275=VERTEX_POINT('',#23129);
#6276=VERTEX_POINT('',#23131);
#6277=VERTEX_POINT('',#23135);
#6278=VERTEX_POINT('',#23137);
#6279=VERTEX_POINT('',#23141);
#6280=VERTEX_POINT('',#23143);
#6281=VERTEX_POINT('',#23147);
#6282=VERTEX_POINT('',#23149);
#6283=VERTEX_POINT('',#23214);
#6284=VERTEX_POINT('',#23216);
#6285=VERTEX_POINT('',#23221);
#6286=VERTEX_POINT('',#23223);
#6287=VERTEX_POINT('',#23226);
#6288=VERTEX_POINT('',#23228);
#6289=VERTEX_POINT('',#23233);
#6290=VERTEX_POINT('',#23237);
#6291=VERTEX_POINT('',#23239);
#6292=VERTEX_POINT('',#23242);
#6293=VERTEX_POINT('',#23244);
#6294=VERTEX_POINT('',#23249);
#6295=VERTEX_POINT('',#23253);
#6296=VERTEX_POINT('',#23256);
#6297=VERTEX_POINT('',#23260);
#6298=VERTEX_POINT('',#23262);
#6299=VERTEX_POINT('',#23272);
#6300=VERTEX_POINT('',#23273);
#6301=VERTEX_POINT('',#23277);
#6302=VERTEX_POINT('',#23278);
#6303=VERTEX_POINT('',#23285);
#6304=VERTEX_POINT('',#23287);
#6305=VERTEX_POINT('',#23306);
#6306=VERTEX_POINT('',#23308);
#6307=VERTEX_POINT('',#23319);
#6308=VERTEX_POINT('',#23351);
#6309=VERTEX_POINT('',#23354);
#6310=VERTEX_POINT('',#23358);
#6311=VERTEX_POINT('',#23361);
#6312=VERTEX_POINT('',#23368);
#6313=VERTEX_POINT('',#23369);
#6314=VERTEX_POINT('',#23371);
#6315=VERTEX_POINT('',#23373);
#6316=VERTEX_POINT('',#23377);
#6317=VERTEX_POINT('',#23379);
#6318=VERTEX_POINT('',#23383);
#6319=VERTEX_POINT('',#23385);
#6320=VERTEX_POINT('',#23389);
#6321=VERTEX_POINT('',#23391);
#6322=VERTEX_POINT('',#23395);
#6323=VERTEX_POINT('',#23397);
#6324=VERTEX_POINT('',#23405);
#6325=VERTEX_POINT('',#23408);
#6326=VERTEX_POINT('',#23412);
#6327=VERTEX_POINT('',#23416);
#6328=EDGE_CURVE('',#5238,#5238,#4470,.T.);
#6329=EDGE_CURVE('',#5238,#5239,#2968,.T.);
#6330=EDGE_CURVE('',#5239,#5239,#4471,.T.);
#6331=EDGE_CURVE('',#5240,#5240,#4472,.T.);
#6332=EDGE_CURVE('',#5240,#5241,#2969,.T.);
#6333=EDGE_CURVE('',#5241,#5241,#4473,.T.);
#6334=EDGE_CURVE('',#5242,#5242,#4474,.T.);
#6335=EDGE_CURVE('',#5242,#5243,#2970,.T.);
#6336=EDGE_CURVE('',#5243,#5243,#4475,.T.);
#6337=EDGE_CURVE('',#5244,#5244,#4476,.T.);
#6338=EDGE_CURVE('',#5244,#5245,#2971,.T.);
#6339=EDGE_CURVE('',#5245,#5245,#4477,.T.);
#6340=EDGE_CURVE('',#5246,#5246,#4478,.T.);
#6341=EDGE_CURVE('',#5246,#5247,#2972,.T.);
#6342=EDGE_CURVE('',#5247,#5247,#4479,.T.);
#6343=EDGE_CURVE('',#5248,#5248,#4480,.T.);
#6344=EDGE_CURVE('',#5248,#5249,#2973,.T.);
#6345=EDGE_CURVE('',#5249,#5249,#4481,.T.);
#6346=EDGE_CURVE('',#5250,#5250,#4482,.T.);
#6347=EDGE_CURVE('',#5250,#5251,#2974,.T.);
#6348=EDGE_CURVE('',#5251,#5251,#4483,.T.);
#6349=EDGE_CURVE('',#5252,#5252,#4484,.T.);
#6350=EDGE_CURVE('',#5252,#5253,#2975,.T.);
#6351=EDGE_CURVE('',#5253,#5253,#4485,.T.);
#6352=EDGE_CURVE('',#5254,#5254,#4486,.T.);
#6353=EDGE_CURVE('',#5254,#5255,#2976,.T.);
#6354=EDGE_CURVE('',#5255,#5255,#4487,.T.);
#6355=EDGE_CURVE('',#5256,#5256,#4488,.T.);
#6356=EDGE_CURVE('',#5256,#5257,#2977,.T.);
#6357=EDGE_CURVE('',#5257,#5257,#4489,.T.);
#6358=EDGE_CURVE('',#5258,#5258,#4490,.T.);
#6359=EDGE_CURVE('',#5258,#5259,#2978,.T.);
#6360=EDGE_CURVE('',#5259,#5259,#4491,.T.);
#6361=EDGE_CURVE('',#5260,#5260,#4492,.T.);
#6362=EDGE_CURVE('',#5260,#5261,#2979,.T.);
#6363=EDGE_CURVE('',#5261,#5261,#4493,.T.);
#6364=EDGE_CURVE('',#5262,#5262,#4494,.T.);
#6365=EDGE_CURVE('',#5262,#5263,#2980,.T.);
#6366=EDGE_CURVE('',#5263,#5263,#4495,.T.);
#6367=EDGE_CURVE('',#5264,#5264,#4496,.T.);
#6368=EDGE_CURVE('',#5264,#5265,#2981,.T.);
#6369=EDGE_CURVE('',#5265,#5265,#4497,.T.);
#6370=EDGE_CURVE('',#5266,#5267,#2982,.T.);
#6371=EDGE_CURVE('',#5267,#5268,#2983,.T.);
#6372=EDGE_CURVE('',#5269,#5268,#2984,.T.);
#6373=EDGE_CURVE('',#5266,#5269,#2985,.T.);
#6374=EDGE_CURVE('',#5270,#5266,#2986,.T.);
#6375=EDGE_CURVE('',#5271,#5269,#2987,.T.);
#6376=EDGE_CURVE('',#5270,#5271,#2988,.T.);
#6377=EDGE_CURVE('',#5272,#5270,#2989,.T.);
#6378=EDGE_CURVE('',#5273,#5271,#2990,.T.);
#6379=EDGE_CURVE('',#5272,#5273,#2991,.T.);
#6380=EDGE_CURVE('',#5267,#5272,#2992,.T.);
#6381=EDGE_CURVE('',#5268,#5273,#2993,.T.);
#6382=EDGE_CURVE('',#5274,#5275,#2994,.T.);
#6383=EDGE_CURVE('',#5275,#5276,#2995,.T.);
#6384=EDGE_CURVE('',#5277,#5276,#2996,.T.);
#6385=EDGE_CURVE('',#5274,#5277,#2997,.T.);
#6386=EDGE_CURVE('',#5278,#5274,#2998,.T.);
#6387=EDGE_CURVE('',#5279,#5277,#2999,.T.);
#6388=EDGE_CURVE('',#5278,#5279,#3000,.T.);
#6389=EDGE_CURVE('',#5280,#5278,#3001,.T.);
#6390=EDGE_CURVE('',#5281,#5279,#3002,.T.);
#6391=EDGE_CURVE('',#5280,#5281,#3003,.T.);
#6392=EDGE_CURVE('',#5275,#5280,#3004,.T.);
#6393=EDGE_CURVE('',#5276,#5281,#3005,.T.);
#6394=EDGE_CURVE('',#5282,#5283,#3006,.T.);
#6395=EDGE_CURVE('',#5283,#5284,#3007,.T.);
#6396=EDGE_CURVE('',#5285,#5284,#3008,.T.);
#6397=EDGE_CURVE('',#5282,#5285,#3009,.T.);
#6398=EDGE_CURVE('',#5286,#5282,#3010,.T.);
#6399=EDGE_CURVE('',#5287,#5285,#3011,.T.);
#6400=EDGE_CURVE('',#5286,#5287,#3012,.T.);
#6401=EDGE_CURVE('',#5288,#5286,#3013,.T.);
#6402=EDGE_CURVE('',#5289,#5287,#3014,.T.);
#6403=EDGE_CURVE('',#5288,#5289,#3015,.T.);
#6404=EDGE_CURVE('',#5283,#5288,#3016,.T.);
#6405=EDGE_CURVE('',#5284,#5289,#3017,.T.);
#6406=EDGE_CURVE('',#5290,#5290,#4498,.T.);
#6407=EDGE_CURVE('',#5290,#5291,#3018,.T.);
#6408=EDGE_CURVE('',#5291,#5291,#4499,.T.);
#6409=EDGE_CURVE('',#5292,#5292,#4500,.T.);
#6410=EDGE_CURVE('',#5292,#5293,#3019,.T.);
#6411=EDGE_CURVE('',#5293,#5293,#4501,.T.);
#6412=EDGE_CURVE('',#5294,#5294,#4502,.T.);
#6413=EDGE_CURVE('',#5294,#5295,#3020,.T.);
#6414=EDGE_CURVE('',#5295,#5295,#4503,.T.);
#6415=EDGE_CURVE('',#5296,#5296,#4504,.T.);
#6416=EDGE_CURVE('',#5296,#5297,#3021,.T.);
#6417=EDGE_CURVE('',#5297,#5297,#4505,.T.);
#6418=EDGE_CURVE('',#5298,#5298,#4506,.T.);
#6419=EDGE_CURVE('',#5298,#5299,#3022,.T.);
#6420=EDGE_CURVE('',#5299,#5299,#4507,.T.);
#6421=EDGE_CURVE('',#5300,#5300,#4508,.T.);
#6422=EDGE_CURVE('',#5300,#5301,#3023,.T.);
#6423=EDGE_CURVE('',#5301,#5301,#4509,.T.);
#6424=EDGE_CURVE('',#5302,#5302,#4510,.T.);
#6425=EDGE_CURVE('',#5302,#5303,#3024,.T.);
#6426=EDGE_CURVE('',#5303,#5303,#4511,.T.);
#6427=EDGE_CURVE('',#5304,#5304,#4512,.T.);
#6428=EDGE_CURVE('',#5304,#5305,#3025,.T.);
#6429=EDGE_CURVE('',#5305,#5305,#4513,.T.);
#6430=EDGE_CURVE('',#5306,#5306,#4514,.T.);
#6431=EDGE_CURVE('',#5306,#5307,#3026,.T.);
#6432=EDGE_CURVE('',#5307,#5307,#4515,.T.);
#6433=EDGE_CURVE('',#5308,#5309,#3027,.T.);
#6434=EDGE_CURVE('',#5310,#5308,#3028,.T.);
#6435=EDGE_CURVE('',#5310,#5311,#3029,.T.);
#6436=EDGE_CURVE('',#5309,#5311,#3030,.T.);
#6437=EDGE_CURVE('',#5312,#5313,#3031,.T.);
#6438=EDGE_CURVE('',#5314,#5312,#3032,.T.);
#6439=EDGE_CURVE('',#5315,#5314,#3033,.T.);
#6440=EDGE_CURVE('',#5313,#5315,#3034,.T.);
#6441=EDGE_CURVE('',#5315,#5316,#3035,.T.);
#6442=EDGE_CURVE('',#5317,#5314,#3036,.T.);
#6443=EDGE_CURVE('',#5316,#5317,#3037,.T.);
#6444=EDGE_CURVE('',#5318,#5310,#3038,.T.);
#6445=EDGE_CURVE('',#5318,#5319,#3039,.T.);
#6446=EDGE_CURVE('',#5311,#5319,#3040,.T.);
#6447=EDGE_CURVE('',#5308,#5320,#3041,.T.);
#6448=EDGE_CURVE('',#5321,#5320,#3042,.T.);
#6449=EDGE_CURVE('',#5313,#5321,#3043,.T.);
#6450=EDGE_CURVE('',#5316,#5318,#3044,.T.);
#6451=EDGE_CURVE('',#5309,#5322,#3045,.T.);
#6452=EDGE_CURVE('',#5320,#5322,#3046,.T.);
#6453=EDGE_CURVE('',#5312,#5323,#3047,.T.);
#6454=EDGE_CURVE('',#5322,#5323,#3048,.T.);
#6455=EDGE_CURVE('',#5319,#5317,#3049,.T.);
#6456=EDGE_CURVE('',#5323,#5321,#3050,.T.);
#6457=EDGE_CURVE('',#5324,#5324,#4516,.T.);
#6458=EDGE_CURVE('',#5324,#5325,#3051,.T.);
#6459=EDGE_CURVE('',#5325,#5325,#4517,.T.);
#6460=EDGE_CURVE('',#5326,#5326,#4518,.T.);
#6461=EDGE_CURVE('',#5326,#5327,#3052,.T.);
#6462=EDGE_CURVE('',#5327,#5327,#4519,.T.);
#6463=EDGE_CURVE('',#5328,#5329,#3053,.T.);
#6464=EDGE_CURVE('',#5330,#5328,#4520,.T.);
#6465=EDGE_CURVE('',#5331,#5330,#3054,.T.);
#6466=EDGE_CURVE('',#5329,#5331,#4521,.T.);
#6467=EDGE_CURVE('',#5332,#5333,#3055,.T.);
#6468=EDGE_CURVE('',#5334,#5332,#4522,.T.);
#6469=EDGE_CURVE('',#5335,#5334,#3056,.T.);
#6470=EDGE_CURVE('',#5333,#5335,#4523,.T.);
#6471=EDGE_CURVE('',#5336,#5337,#3057,.T.);
#6472=EDGE_CURVE('',#5338,#5336,#4524,.T.);
#6473=EDGE_CURVE('',#5339,#5338,#3058,.T.);
#6474=EDGE_CURVE('',#5337,#5339,#4525,.T.);
#6475=EDGE_CURVE('',#5340,#5341,#3059,.T.);
#6476=EDGE_CURVE('',#5342,#5340,#4526,.T.);
#6477=EDGE_CURVE('',#5343,#5342,#3060,.T.);
#6478=EDGE_CURVE('',#5341,#5343,#4527,.T.);
#6479=EDGE_CURVE('',#5342,#5328,#4528,.T.);
#6480=EDGE_CURVE('',#5338,#5340,#4529,.T.);
#6481=EDGE_CURVE('',#5334,#5336,#4530,.T.);
#6482=EDGE_CURVE('',#5330,#5332,#4531,.T.);
#6483=EDGE_CURVE('',#5344,#5344,#4532,.T.);
#6484=EDGE_CURVE('',#5339,#5341,#4533,.T.);
#6485=EDGE_CURVE('',#5335,#5337,#4534,.T.);
#6486=EDGE_CURVE('',#5343,#5329,#4535,.T.);
#6487=EDGE_CURVE('',#5331,#5333,#4536,.T.);
#6488=EDGE_CURVE('',#5345,#5345,#4537,.T.);
#6489=EDGE_CURVE('',#5345,#5346,#3061,.T.);
#6490=EDGE_CURVE('',#5346,#5346,#4538,.T.);
#6491=EDGE_CURVE('',#5347,#5347,#4539,.T.);
#6492=EDGE_CURVE('',#5347,#5344,#3062,.T.);
#6493=EDGE_CURVE('',#5348,#5349,#3063,.T.);
#6494=EDGE_CURVE('',#5350,#5348,#4540,.T.);
#6495=EDGE_CURVE('',#5351,#5350,#3064,.T.);
#6496=EDGE_CURVE('',#5349,#5351,#4541,.T.);
#6497=EDGE_CURVE('',#5352,#5353,#3065,.T.);
#6498=EDGE_CURVE('',#5354,#5352,#4542,.T.);
#6499=EDGE_CURVE('',#5355,#5354,#3066,.T.);
#6500=EDGE_CURVE('',#5353,#5355,#4543,.T.);
#6501=EDGE_CURVE('',#5356,#5357,#3067,.T.);
#6502=EDGE_CURVE('',#5358,#5356,#4544,.T.);
#6503=EDGE_CURVE('',#5359,#5358,#3068,.T.);
#6504=EDGE_CURVE('',#5357,#5359,#4545,.T.);
#6505=EDGE_CURVE('',#5360,#5361,#3069,.T.);
#6506=EDGE_CURVE('',#5362,#5360,#4546,.T.);
#6507=EDGE_CURVE('',#5363,#5362,#3070,.T.);
#6508=EDGE_CURVE('',#5361,#5363,#4547,.T.);
#6509=EDGE_CURVE('',#5362,#5348,#4548,.T.);
#6510=EDGE_CURVE('',#5358,#5360,#4549,.T.);
#6511=EDGE_CURVE('',#5354,#5356,#4550,.T.);
#6512=EDGE_CURVE('',#5350,#5352,#4551,.T.);
#6513=EDGE_CURVE('',#5364,#5364,#4552,.T.);
#6514=EDGE_CURVE('',#5359,#5361,#4553,.T.);
#6515=EDGE_CURVE('',#5355,#5357,#4554,.T.);
#6516=EDGE_CURVE('',#5363,#5349,#4555,.T.);
#6517=EDGE_CURVE('',#5351,#5353,#4556,.T.);
#6518=EDGE_CURVE('',#5364,#5365,#3071,.T.);
#6519=EDGE_CURVE('',#5365,#5365,#4557,.T.);
#6520=EDGE_CURVE('',#5366,#5366,#4558,.T.);
#6521=EDGE_CURVE('',#5367,#5367,#4559,.T.);
#6522=EDGE_CURVE('',#5367,#5366,#3072,.T.);
#6523=EDGE_CURVE('',#5368,#5368,#4560,.T.);
#6524=EDGE_CURVE('',#5368,#5369,#3073,.T.);
#6525=EDGE_CURVE('',#5369,#5369,#4561,.T.);
#6526=EDGE_CURVE('',#5370,#5370,#4562,.T.);
#6527=EDGE_CURVE('',#5371,#5371,#4563,.T.);
#6528=EDGE_CURVE('',#5371,#5372,#3074,.T.);
#6529=EDGE_CURVE('',#5372,#5372,#4564,.T.);
#6530=EDGE_CURVE('',#5373,#5373,#4565,.T.);
#6531=EDGE_CURVE('',#5374,#5374,#4566,.T.);
#6532=EDGE_CURVE('',#5374,#5370,#3075,.T.);
#6533=EDGE_CURVE('',#5375,#5375,#4567,.T.);
#6534=EDGE_CURVE('',#5375,#5373,#3076,.T.);
#6535=EDGE_CURVE('',#5376,#5376,#4568,.T.);
#6536=EDGE_CURVE('',#5376,#5377,#3077,.T.);
#6537=EDGE_CURVE('',#5377,#5377,#4569,.T.);
#6538=EDGE_CURVE('',#5378,#5379,#3078,.T.);
#6539=EDGE_CURVE('',#5379,#5380,#3079,.T.);
#6540=EDGE_CURVE('',#5381,#5380,#3080,.T.);
#6541=EDGE_CURVE('',#5378,#5381,#3081,.T.);
#6542=EDGE_CURVE('',#5382,#5378,#3082,.T.);
#6543=EDGE_CURVE('',#5383,#5381,#3083,.T.);
#6544=EDGE_CURVE('',#5382,#5383,#3084,.T.);
#6545=EDGE_CURVE('',#5384,#5382,#3085,.T.);
#6546=EDGE_CURVE('',#5385,#5383,#3086,.T.);
#6547=EDGE_CURVE('',#5384,#5385,#3087,.T.);
#6548=EDGE_CURVE('',#5379,#5384,#3088,.T.);
#6549=EDGE_CURVE('',#5380,#5385,#3089,.T.);
#6550=EDGE_CURVE('',#5386,#5386,#4570,.T.);
#6551=EDGE_CURVE('',#5386,#5387,#3090,.T.);
#6552=EDGE_CURVE('',#5387,#5387,#4571,.T.);
#6553=EDGE_CURVE('',#5388,#5388,#4572,.T.);
#6554=EDGE_CURVE('',#5388,#5389,#3091,.T.);
#6555=EDGE_CURVE('',#5389,#5389,#4573,.T.);
#6556=EDGE_CURVE('',#5390,#5390,#4574,.T.);
#6557=EDGE_CURVE('',#5390,#5391,#3092,.T.);
#6558=EDGE_CURVE('',#5391,#5391,#4575,.T.);
#6559=EDGE_CURVE('',#5392,#5392,#4576,.T.);
#6560=EDGE_CURVE('',#5393,#5393,#4577,.T.);
#6561=EDGE_CURVE('',#5393,#5394,#3093,.T.);
#6562=EDGE_CURVE('',#5394,#5394,#4578,.T.);
#6563=EDGE_CURVE('',#5395,#5395,#4579,.T.);
#6564=EDGE_CURVE('',#5396,#5396,#4580,.T.);
#6565=EDGE_CURVE('',#5396,#5392,#3094,.T.);
#6566=EDGE_CURVE('',#5397,#5397,#4581,.T.);
#6567=EDGE_CURVE('',#5397,#5395,#3095,.T.);
#6568=EDGE_CURVE('',#5398,#5398,#4582,.T.);
#6569=EDGE_CURVE('',#5398,#5399,#3096,.T.);
#6570=EDGE_CURVE('',#5399,#5399,#4583,.T.);
#6571=EDGE_CURVE('',#5400,#5401,#3097,.T.);
#6572=EDGE_CURVE('',#5401,#5402,#3098,.T.);
#6573=EDGE_CURVE('',#5403,#5402,#3099,.T.);
#6574=EDGE_CURVE('',#5400,#5403,#3100,.T.);
#6575=EDGE_CURVE('',#5404,#5400,#3101,.T.);
#6576=EDGE_CURVE('',#5405,#5403,#3102,.T.);
#6577=EDGE_CURVE('',#5404,#5405,#3103,.T.);
#6578=EDGE_CURVE('',#5406,#5404,#3104,.T.);
#6579=EDGE_CURVE('',#5407,#5405,#3105,.T.);
#6580=EDGE_CURVE('',#5406,#5407,#3106,.T.);
#6581=EDGE_CURVE('',#5401,#5406,#3107,.T.);
#6582=EDGE_CURVE('',#5402,#5407,#3108,.T.);
#6583=EDGE_CURVE('',#5408,#5408,#4584,.T.);
#6584=EDGE_CURVE('',#5408,#5409,#3109,.T.);
#6585=EDGE_CURVE('',#5409,#5409,#4585,.T.);
#6586=EDGE_CURVE('',#5410,#5410,#4586,.T.);
#6587=EDGE_CURVE('',#5410,#5411,#3110,.T.);
#6588=EDGE_CURVE('',#5411,#5411,#4587,.T.);
#6589=EDGE_CURVE('',#5412,#5412,#4588,.T.);
#6590=EDGE_CURVE('',#5412,#5413,#3111,.T.);
#6591=EDGE_CURVE('',#5413,#5413,#4589,.T.);
#6592=EDGE_CURVE('',#5414,#5414,#4590,.T.);
#6593=EDGE_CURVE('',#5414,#5415,#3112,.T.);
#6594=EDGE_CURVE('',#5415,#5415,#4591,.T.);
#6595=EDGE_CURVE('',#5416,#5417,#3113,.T.);
#6596=EDGE_CURVE('',#5418,#5416,#4592,.T.);
#6597=EDGE_CURVE('',#5418,#5419,#3114,.T.);
#6598=EDGE_CURVE('',#5420,#5419,#4593,.T.);
#6599=EDGE_CURVE('',#5417,#5420,#491,.T.);
#6600=EDGE_CURVE('',#5421,#5422,#3115,.T.);
#6601=EDGE_CURVE('',#5423,#5421,#4594,.T.);
#6602=EDGE_CURVE('',#5423,#5424,#3116,.T.);
#6603=EDGE_CURVE('',#5425,#5424,#4595,.T.);
#6604=EDGE_CURVE('',#5422,#5425,#492,.T.);
#6605=EDGE_CURVE('',#5426,#5422,#493,.T.);
#6606=EDGE_CURVE('',#5424,#5426,#4596,.T.);
#6607=EDGE_CURVE('',#5423,#5424,#3117,.T.);
#6608=EDGE_CURVE('',#5421,#5423,#4597,.T.);
#6609=EDGE_CURVE('',#5427,#5427,#4598,.T.);
#6610=EDGE_CURVE('',#5428,#5417,#494,.T.);
#6611=EDGE_CURVE('',#5419,#5428,#4599,.T.);
#6612=EDGE_CURVE('',#5418,#5419,#3118,.T.);
#6613=EDGE_CURVE('',#5416,#5418,#4600,.T.);
#6614=EDGE_CURVE('',#5429,#5429,#4601,.T.);
#6615=EDGE_CURVE('',#5426,#5430,#3119,.T.);
#6616=EDGE_CURVE('',#5430,#5431,#3120,.T.);
#6617=EDGE_CURVE('',#5431,#5424,#3121,.T.);
#6618=EDGE_CURVE('',#5428,#5432,#3122,.T.);
#6619=EDGE_CURVE('',#5432,#5433,#3123,.T.);
#6620=EDGE_CURVE('',#5433,#5419,#3124,.T.);
#6621=EDGE_CURVE('',#5419,#5434,#3125,.T.);
#6622=EDGE_CURVE('',#5434,#5435,#3126,.T.);
#6623=EDGE_CURVE('',#5435,#5420,#3127,.T.);
#6624=EDGE_CURVE('',#5436,#5436,#4602,.T.);
#6625=EDGE_CURVE('',#5436,#5427,#3128,.T.);
#6626=EDGE_CURVE('',#5437,#5437,#4603,.T.);
#6627=EDGE_CURVE('',#5437,#5429,#3129,.T.);
#6628=EDGE_CURVE('',#5438,#5425,#3130,.T.);
#6629=EDGE_CURVE('',#5432,#5438,#4604,.T.);
#6630=EDGE_CURVE('',#5430,#5435,#4605,.T.);
#6631=EDGE_CURVE('',#5439,#5438,#3131,.T.);
#6632=EDGE_CURVE('',#5440,#5439,#3132,.T.);
#6633=EDGE_CURVE('',#5440,#5441,#3133,.T.);
#6634=EDGE_CURVE('',#5441,#5433,#3134,.T.);
#6635=EDGE_CURVE('',#5424,#5439,#3135,.T.);
#6636=EDGE_CURVE('',#5441,#5442,#3136,.T.);
#6637=EDGE_CURVE('',#5442,#5434,#3137,.T.);
#6638=EDGE_CURVE('',#5443,#5440,#3138,.T.);
#6639=EDGE_CURVE('',#5443,#5431,#3139,.T.);
#6640=EDGE_CURVE('',#5442,#5443,#3140,.T.);
#6641=EDGE_CURVE('',#5444,#5444,#4606,.T.);
#6642=EDGE_CURVE('',#5444,#5445,#3141,.T.);
#6643=EDGE_CURVE('',#5445,#5445,#4607,.T.);
#6644=EDGE_CURVE('',#5446,#5446,#4608,.T.);
#6645=EDGE_CURVE('',#5447,#5447,#4609,.T.);
#6646=EDGE_CURVE('',#5447,#5448,#3142,.T.);
#6647=EDGE_CURVE('',#5448,#5448,#4610,.T.);
#6648=EDGE_CURVE('',#5449,#5449,#4611,.T.);
#6649=EDGE_CURVE('',#5450,#5450,#4612,.T.);
#6650=EDGE_CURVE('',#5450,#5451,#3143,.T.);
#6651=EDGE_CURVE('',#5451,#5451,#4613,.T.);
#6652=EDGE_CURVE('',#5452,#5452,#4614,.T.);
#6653=EDGE_CURVE('',#5453,#5453,#4615,.T.);
#6654=EDGE_CURVE('',#5453,#5454,#3144,.T.);
#6655=EDGE_CURVE('',#5454,#5454,#4616,.T.);
#6656=EDGE_CURVE('',#5455,#5455,#4617,.T.);
#6657=EDGE_CURVE('',#5456,#5456,#4618,.T.);
#6658=EDGE_CURVE('',#5456,#5446,#3145,.T.);
#6659=EDGE_CURVE('',#5457,#5457,#4619,.T.);
#6660=EDGE_CURVE('',#5457,#5449,#3146,.T.);
#6661=EDGE_CURVE('',#5458,#5458,#4620,.T.);
#6662=EDGE_CURVE('',#5458,#5452,#3147,.T.);
#6663=EDGE_CURVE('',#5459,#5459,#4621,.T.);
#6664=EDGE_CURVE('',#5459,#5455,#3148,.T.);
#6665=EDGE_CURVE('',#5460,#5461,#3149,.T.);
#6666=EDGE_CURVE('',#5461,#5462,#3150,.T.);
#6667=EDGE_CURVE('',#5463,#5462,#3151,.T.);
#6668=EDGE_CURVE('',#5460,#5463,#3152,.T.);
#6669=EDGE_CURVE('',#5464,#5460,#3153,.T.);
#6670=EDGE_CURVE('',#5465,#5463,#3154,.T.);
#6671=EDGE_CURVE('',#5464,#5465,#3155,.T.);
#6672=EDGE_CURVE('',#5466,#5464,#3156,.T.);
#6673=EDGE_CURVE('',#5467,#5465,#3157,.T.);
#6674=EDGE_CURVE('',#5466,#5467,#3158,.T.);
#6675=EDGE_CURVE('',#5468,#5466,#3159,.T.);
#6676=EDGE_CURVE('',#5469,#5467,#3160,.T.);
#6677=EDGE_CURVE('',#5468,#5469,#3161,.T.);
#6678=EDGE_CURVE('',#5470,#5468,#3162,.T.);
#6679=EDGE_CURVE('',#5471,#5469,#3163,.T.);
#6680=EDGE_CURVE('',#5470,#5471,#3164,.T.);
#6681=EDGE_CURVE('',#5472,#5470,#3165,.T.);
#6682=EDGE_CURVE('',#5473,#5471,#3166,.T.);
#6683=EDGE_CURVE('',#5472,#5473,#3167,.T.);
#6684=EDGE_CURVE('',#5474,#5472,#3168,.T.);
#6685=EDGE_CURVE('',#5475,#5473,#3169,.T.);
#6686=EDGE_CURVE('',#5474,#5475,#3170,.T.);
#6687=EDGE_CURVE('',#5476,#5474,#3171,.T.);
#6688=EDGE_CURVE('',#5477,#5475,#3172,.T.);
#6689=EDGE_CURVE('',#5476,#5477,#3173,.T.);
#6690=EDGE_CURVE('',#5478,#5476,#3174,.T.);
#6691=EDGE_CURVE('',#5479,#5477,#3175,.T.);
#6692=EDGE_CURVE('',#5478,#5479,#3176,.T.);
#6693=EDGE_CURVE('',#5480,#5478,#3177,.T.);
#6694=EDGE_CURVE('',#5481,#5479,#3178,.T.);
#6695=EDGE_CURVE('',#5480,#5481,#3179,.T.);
#6696=EDGE_CURVE('',#5482,#5480,#3180,.T.);
#6697=EDGE_CURVE('',#5483,#5481,#3181,.T.);
#6698=EDGE_CURVE('',#5482,#5483,#3182,.T.);
#6699=EDGE_CURVE('',#5461,#5482,#3183,.T.);
#6700=EDGE_CURVE('',#5462,#5483,#3184,.T.);
#6701=EDGE_CURVE('',#5484,#5485,#4622,.T.);
#6702=EDGE_CURVE('',#5485,#5484,#4623,.T.);
#6703=EDGE_CURVE('',#5485,#5486,#4624,.T.);
#6704=EDGE_CURVE('',#5487,#5486,#4625,.T.);
#6705=EDGE_CURVE('',#5486,#5487,#4626,.T.);
#6706=EDGE_CURVE('',#5487,#5488,#3185,.T.);
#6707=EDGE_CURVE('',#5488,#5488,#4627,.T.);
#6708=EDGE_CURVE('',#5489,#5489,#4628,.T.);
#6709=EDGE_CURVE('',#5489,#5490,#3186,.T.);
#6710=EDGE_CURVE('',#5490,#5490,#4629,.T.);
#6711=EDGE_CURVE('',#5490,#5491,#3187,.T.);
#6712=EDGE_CURVE('',#5491,#5491,#4630,.T.);
#6713=EDGE_CURVE('',#5492,#5492,#4631,.T.);
#6714=EDGE_CURVE('',#5492,#5484,#3188,.T.);
#6715=EDGE_CURVE('',#5493,#5493,#4632,.T.);
#6716=EDGE_CURVE('',#5493,#5489,#3189,.T.);
#6717=EDGE_CURVE('',#5494,#5495,#4633,.T.);
#6718=EDGE_CURVE('',#5495,#5494,#4634,.T.);
#6719=EDGE_CURVE('',#5495,#5496,#4635,.T.);
#6720=EDGE_CURVE('',#5497,#5496,#4636,.T.);
#6721=EDGE_CURVE('',#5496,#5497,#4637,.T.);
#6722=EDGE_CURVE('',#5498,#5498,#4638,.T.);
#6723=EDGE_CURVE('',#5498,#5497,#3190,.T.);
#6724=EDGE_CURVE('',#5499,#5499,#4639,.T.);
#6725=EDGE_CURVE('',#5500,#5500,#4640,.T.);
#6726=EDGE_CURVE('',#5501,#5501,#4641,.T.);
#6727=EDGE_CURVE('',#5501,#5499,#3191,.T.);
#6728=EDGE_CURVE('',#5502,#5502,#4642,.T.);
#6729=EDGE_CURVE('',#5502,#5501,#3192,.T.);
#6730=EDGE_CURVE('',#5503,#5503,#4643,.T.);
#6731=EDGE_CURVE('',#5503,#5502,#3193,.T.);
#6732=EDGE_CURVE('',#5494,#5500,#3194,.T.);
#6733=EDGE_CURVE('',#5504,#5505,#4644,.T.);
#6734=EDGE_CURVE('',#5506,#5507,#4645,.T.);
#6735=EDGE_CURVE('',#5508,#5509,#4646,.T.);
#6736=EDGE_CURVE('',#5510,#5511,#4647,.T.);
#6737=EDGE_CURVE('',#5512,#5513,#4648,.T.);
#6738=EDGE_CURVE('',#5514,#5515,#4649,.T.);
#6739=EDGE_CURVE('',#5516,#5517,#4650,.T.);
#6740=EDGE_CURVE('',#5518,#5519,#4651,.T.);
#6741=EDGE_CURVE('',#5520,#5521,#495,.T.);
#6742=EDGE_CURVE('',#5522,#5520,#4652,.T.);
#6743=EDGE_CURVE('',#5523,#5522,#496,.T.);
#6744=EDGE_CURVE('',#5521,#5523,#4653,.T.);
#6745=EDGE_CURVE('',#5524,#5522,#4654,.T.);
#6746=EDGE_CURVE('',#5524,#5525,#497,.T.);
#6747=EDGE_CURVE('',#5526,#5525,#4655,.T.);
#6748=EDGE_CURVE('',#5526,#5527,#498,.T.);
#6749=EDGE_CURVE('',#5528,#5527,#4656,.T.);
#6750=EDGE_CURVE('',#5528,#5529,#499,.T.);
#6751=EDGE_CURVE('',#5529,#5530,#3195,.T.);
#6752=EDGE_CURVE('',#5530,#5530,#4657,.T.);
#6753=EDGE_CURVE('',#5529,#5531,#500,.T.);
#6754=EDGE_CURVE('',#5532,#5531,#4658,.T.);
#6755=EDGE_CURVE('',#5532,#5533,#501,.T.);
#6756=EDGE_CURVE('',#5534,#5533,#4659,.T.);
#6757=EDGE_CURVE('',#5534,#5535,#502,.T.);
#6758=EDGE_CURVE('',#5536,#5535,#4660,.T.);
#6759=EDGE_CURVE('',#5536,#5537,#503,.T.);
#6760=EDGE_CURVE('',#5538,#5537,#4661,.T.);
#6761=EDGE_CURVE('',#5538,#5539,#504,.T.);
#6762=EDGE_CURVE('',#5523,#5539,#4662,.T.);
#6763=EDGE_CURVE('',#5520,#5540,#4663,.T.);
#6764=EDGE_CURVE('',#5540,#5524,#4664,.T.);
#6765=EDGE_CURVE('',#5541,#5540,#505,.T.);
#6766=EDGE_CURVE('',#5525,#5541,#4665,.T.);
#6767=EDGE_CURVE('',#5541,#5542,#4666,.T.);
#6768=EDGE_CURVE('',#5542,#5526,#4667,.T.);
#6769=EDGE_CURVE('',#5543,#5542,#506,.T.);
#6770=EDGE_CURVE('',#5527,#5543,#4668,.T.);
#6771=EDGE_CURVE('',#5543,#5544,#4669,.T.);
#6772=EDGE_CURVE('',#5544,#5528,#4670,.T.);
#6773=EDGE_CURVE('',#5545,#5546,#507,.T.);
#6774=EDGE_CURVE('',#5531,#5545,#4671,.T.);
#6775=EDGE_CURVE('',#5546,#5544,#508,.T.);
#6776=EDGE_CURVE('',#5545,#5547,#4672,.T.);
#6777=EDGE_CURVE('',#5547,#5532,#4673,.T.);
#6778=EDGE_CURVE('',#5548,#5547,#509,.T.);
#6779=EDGE_CURVE('',#5533,#5548,#4674,.T.);
#6780=EDGE_CURVE('',#5548,#5549,#4675,.T.);
#6781=EDGE_CURVE('',#5549,#5534,#4676,.T.);
#6782=EDGE_CURVE('',#5550,#5549,#510,.T.);
#6783=EDGE_CURVE('',#5535,#5550,#4677,.T.);
#6784=EDGE_CURVE('',#5550,#5551,#4678,.T.);
#6785=EDGE_CURVE('',#5551,#5536,#4679,.T.);
#6786=EDGE_CURVE('',#5552,#5551,#511,.T.);
#6787=EDGE_CURVE('',#5537,#5552,#4680,.T.);
#6788=EDGE_CURVE('',#5553,#5553,#4681,.T.);
#6789=EDGE_CURVE('',#5553,#5546,#3196,.T.);
#6790=EDGE_CURVE('',#5554,#5521,#4682,.T.);
#6791=EDGE_CURVE('',#5554,#5555,#512,.T.);
#6792=EDGE_CURVE('',#5552,#5555,#4683,.T.);
#6793=EDGE_CURVE('',#5539,#5554,#4684,.T.);
#6794=EDGE_CURVE('',#5555,#5538,#4685,.T.);
#6795=EDGE_CURVE('',#5556,#5556,#4686,.T.);
#6796=EDGE_CURVE('',#5557,#5557,#4687,.T.);
#6797=EDGE_CURVE('',#5558,#5558,#4688,.T.);
#6798=EDGE_CURVE('',#5558,#5556,#3197,.T.);
#6799=EDGE_CURVE('',#5559,#5559,#4689,.T.);
#6800=EDGE_CURVE('',#5559,#5557,#3198,.T.);
#6801=EDGE_CURVE('',#5560,#5560,#4690,.T.);
#6802=EDGE_CURVE('',#5561,#5561,#4691,.T.);
#6803=EDGE_CURVE('',#5562,#5562,#4692,.T.);
#6804=EDGE_CURVE('',#5562,#5560,#3199,.T.);
#6805=EDGE_CURVE('',#5563,#5563,#4693,.T.);
#6806=EDGE_CURVE('',#5563,#5561,#3200,.T.);
#6807=EDGE_CURVE('',#5564,#5564,#4694,.T.);
#6808=EDGE_CURVE('',#5564,#5565,#3201,.T.);
#6809=EDGE_CURVE('',#5565,#5565,#4695,.T.);
#6810=EDGE_CURVE('',#5566,#5566,#4696,.T.);
#6811=EDGE_CURVE('',#5566,#5567,#3202,.T.);
#6812=EDGE_CURVE('',#5567,#5567,#4697,.T.);
#6813=EDGE_CURVE('',#5568,#5568,#4698,.T.);
#6814=EDGE_CURVE('',#5568,#5569,#3203,.T.);
#6815=EDGE_CURVE('',#5569,#5569,#4699,.T.);
#6816=EDGE_CURVE('',#5570,#5570,#4700,.T.);
#6817=EDGE_CURVE('',#5570,#5571,#3204,.T.);
#6818=EDGE_CURVE('',#5571,#5571,#4701,.T.);
#6819=EDGE_CURVE('',#5572,#5572,#4702,.T.);
#6820=EDGE_CURVE('',#5572,#5573,#3205,.T.);
#6821=EDGE_CURVE('',#5573,#5573,#4703,.T.);
#6822=EDGE_CURVE('',#5574,#5574,#4704,.T.);
#6823=EDGE_CURVE('',#5574,#5575,#3206,.T.);
#6824=EDGE_CURVE('',#5575,#5575,#4705,.T.);
#6825=EDGE_CURVE('',#5576,#5576,#4706,.T.);
#6826=EDGE_CURVE('',#5576,#5577,#3207,.T.);
#6827=EDGE_CURVE('',#5577,#5577,#4707,.T.);
#6828=EDGE_CURVE('',#5578,#5578,#4708,.T.);
#6829=EDGE_CURVE('',#5578,#5579,#3208,.T.);
#6830=EDGE_CURVE('',#5579,#5579,#4709,.T.);
#6831=EDGE_CURVE('',#5580,#5580,#4710,.T.);
#6832=EDGE_CURVE('',#5580,#5581,#3209,.T.);
#6833=EDGE_CURVE('',#5581,#5581,#4711,.T.);
#6834=EDGE_CURVE('',#5582,#5582,#4712,.T.);
#6835=EDGE_CURVE('',#5582,#5583,#3210,.T.);
#6836=EDGE_CURVE('',#5583,#5583,#4713,.T.);
#6837=EDGE_CURVE('',#5584,#5585,#3211,.T.);
#6838=EDGE_CURVE('',#5585,#5586,#3212,.T.);
#6839=EDGE_CURVE('',#5587,#5586,#3213,.T.);
#6840=EDGE_CURVE('',#5584,#5587,#3214,.T.);
#6841=EDGE_CURVE('',#5588,#5584,#3215,.T.);
#6842=EDGE_CURVE('',#5589,#5587,#3216,.T.);
#6843=EDGE_CURVE('',#5588,#5589,#3217,.T.);
#6844=EDGE_CURVE('',#5590,#5588,#3218,.T.);
#6845=EDGE_CURVE('',#5591,#5589,#3219,.T.);
#6846=EDGE_CURVE('',#5590,#5591,#3220,.T.);
#6847=EDGE_CURVE('',#5585,#5590,#3221,.T.);
#6848=EDGE_CURVE('',#5586,#5591,#3222,.T.);
#6849=EDGE_CURVE('',#5592,#5592,#4714,.T.);
#6850=EDGE_CURVE('',#5592,#5593,#3223,.T.);
#6851=EDGE_CURVE('',#5593,#5593,#4715,.T.);
#6852=EDGE_CURVE('',#5594,#5594,#4716,.T.);
#6853=EDGE_CURVE('',#5594,#5595,#3224,.T.);
#6854=EDGE_CURVE('',#5595,#5595,#4717,.T.);
#6855=EDGE_CURVE('',#5596,#5596,#4718,.T.);
#6856=EDGE_CURVE('',#5596,#5597,#3225,.T.);
#6857=EDGE_CURVE('',#5597,#5597,#4719,.T.);
#6858=EDGE_CURVE('',#5598,#5598,#4720,.T.);
#6859=EDGE_CURVE('',#5598,#5599,#3226,.T.);
#6860=EDGE_CURVE('',#5599,#5599,#4721,.T.);
#6861=EDGE_CURVE('',#5600,#5600,#4722,.T.);
#6862=EDGE_CURVE('',#5600,#5601,#3227,.T.);
#6863=EDGE_CURVE('',#5601,#5601,#4723,.T.);
#6864=EDGE_CURVE('',#5602,#5603,#3228,.T.);
#6865=EDGE_CURVE('',#5603,#5602,#4724,.T.);
#6866=EDGE_CURVE('',#5604,#5602,#3229,.T.);
#6867=EDGE_CURVE('',#5605,#5604,#4725,.T.);
#6868=EDGE_CURVE('',#5603,#5605,#3230,.T.);
#6869=EDGE_CURVE('',#5606,#5607,#3231,.T.);
#6870=EDGE_CURVE('',#5607,#5606,#4726,.T.);
#6871=EDGE_CURVE('',#5608,#5606,#3232,.T.);
#6872=EDGE_CURVE('',#5609,#5608,#4727,.T.);
#6873=EDGE_CURVE('',#5607,#5609,#3233,.T.);
#6874=EDGE_CURVE('',#5610,#5611,#3234,.T.);
#6875=EDGE_CURVE('',#5611,#5610,#4728,.T.);
#6876=EDGE_CURVE('',#5612,#5610,#3235,.T.);
#6877=EDGE_CURVE('',#5613,#5612,#4729,.T.);
#6878=EDGE_CURVE('',#5611,#5613,#3236,.T.);
#6879=EDGE_CURVE('',#5614,#5615,#3237,.T.);
#6880=EDGE_CURVE('',#5615,#5614,#4730,.T.);
#6881=EDGE_CURVE('',#5616,#5614,#3238,.T.);
#6882=EDGE_CURVE('',#5617,#5616,#4731,.T.);
#6883=EDGE_CURVE('',#5615,#5617,#3239,.T.);
#6884=EDGE_CURVE('',#5605,#5618,#3240,.T.);
#6885=EDGE_CURVE('',#5618,#5619,#3241,.T.);
#6886=EDGE_CURVE('',#5619,#5620,#3242,.T.);
#6887=EDGE_CURVE('',#5620,#5621,#3243,.T.);
#6888=EDGE_CURVE('',#5622,#5621,#3244,.T.);
#6889=EDGE_CURVE('',#5623,#5622,#3245,.T.);
#6890=EDGE_CURVE('',#5623,#5624,#3246,.T.);
#6891=EDGE_CURVE('',#5624,#5625,#3247,.T.);
#6892=EDGE_CURVE('',#5625,#5612,#3248,.T.);
#6893=EDGE_CURVE('',#5613,#5604,#3249,.T.);
#6894=EDGE_CURVE('',#5609,#5626,#3250,.T.);
#6895=EDGE_CURVE('',#5626,#5627,#3251,.T.);
#6896=EDGE_CURVE('',#5627,#5628,#3252,.T.);
#6897=EDGE_CURVE('',#5628,#5629,#3253,.T.);
#6898=EDGE_CURVE('',#5630,#5629,#3254,.T.);
#6899=EDGE_CURVE('',#5631,#5630,#3255,.T.);
#6900=EDGE_CURVE('',#5631,#5632,#3256,.T.);
#6901=EDGE_CURVE('',#5632,#5633,#3257,.T.);
#6902=EDGE_CURVE('',#5633,#5616,#3258,.T.);
#6903=EDGE_CURVE('',#5617,#5608,#3259,.T.);
#6904=EDGE_CURVE('',#5634,#5634,#4732,.T.);
#6905=EDGE_CURVE('',#5634,#5635,#3260,.T.);
#6906=EDGE_CURVE('',#5635,#5635,#4733,.T.);
#6907=EDGE_CURVE('',#5636,#5636,#4734,.T.);
#6908=EDGE_CURVE('',#5636,#5637,#3261,.T.);
#6909=EDGE_CURVE('',#5637,#5637,#4735,.T.);
#6910=EDGE_CURVE('',#5638,#5638,#4736,.T.);
#6911=EDGE_CURVE('',#5638,#5639,#3262,.T.);
#6912=EDGE_CURVE('',#5639,#5639,#4737,.T.);
#6913=EDGE_CURVE('',#5640,#5640,#4738,.T.);
#6914=EDGE_CURVE('',#5640,#5641,#3263,.T.);
#6915=EDGE_CURVE('',#5641,#5641,#4739,.T.);
#6916=EDGE_CURVE('',#5620,#5631,#3264,.T.);
#6917=EDGE_CURVE('',#5619,#5632,#3265,.T.);
#6918=EDGE_CURVE('',#5628,#5623,#3266,.T.);
#6919=EDGE_CURVE('',#5624,#5627,#3267,.T.);
#6920=EDGE_CURVE('',#5625,#5626,#3268,.T.);
#6921=EDGE_CURVE('',#5618,#5633,#3269,.T.);
#6922=EDGE_CURVE('',#5621,#5630,#3270,.T.);
#6923=EDGE_CURVE('',#5629,#5622,#3271,.T.);
#6924=EDGE_CURVE('',#5642,#5642,#4740,.T.);
#6925=EDGE_CURVE('',#5642,#5643,#3272,.T.);
#6926=EDGE_CURVE('',#5643,#5643,#4741,.T.);
#6927=EDGE_CURVE('',#5644,#5644,#4742,.T.);
#6928=EDGE_CURVE('',#5644,#5645,#3273,.T.);
#6929=EDGE_CURVE('',#5645,#5645,#4743,.T.);
#6930=EDGE_CURVE('',#5646,#5647,#3274,.T.);
#6931=EDGE_CURVE('',#5648,#5646,#4744,.T.);
#6932=EDGE_CURVE('',#5649,#5648,#3275,.T.);
#6933=EDGE_CURVE('',#5647,#5649,#4745,.T.);
#6934=EDGE_CURVE('',#5650,#5651,#3276,.T.);
#6935=EDGE_CURVE('',#5652,#5650,#4746,.T.);
#6936=EDGE_CURVE('',#5653,#5652,#3277,.T.);
#6937=EDGE_CURVE('',#5651,#5653,#4747,.T.);
#6938=EDGE_CURVE('',#5654,#5655,#3278,.T.);
#6939=EDGE_CURVE('',#5656,#5654,#4748,.T.);
#6940=EDGE_CURVE('',#5657,#5656,#3279,.T.);
#6941=EDGE_CURVE('',#5655,#5657,#4749,.T.);
#6942=EDGE_CURVE('',#5658,#5659,#3280,.T.);
#6943=EDGE_CURVE('',#5660,#5658,#4750,.T.);
#6944=EDGE_CURVE('',#5661,#5660,#3281,.T.);
#6945=EDGE_CURVE('',#5659,#5661,#4751,.T.);
#6946=EDGE_CURVE('',#5660,#5646,#4752,.T.);
#6947=EDGE_CURVE('',#5656,#5658,#4753,.T.);
#6948=EDGE_CURVE('',#5652,#5654,#4754,.T.);
#6949=EDGE_CURVE('',#5648,#5650,#4755,.T.);
#6950=EDGE_CURVE('',#5662,#5662,#4756,.T.);
#6951=EDGE_CURVE('',#5657,#5659,#4757,.T.);
#6952=EDGE_CURVE('',#5653,#5655,#4758,.T.);
#6953=EDGE_CURVE('',#5661,#5647,#4759,.T.);
#6954=EDGE_CURVE('',#5649,#5651,#4760,.T.);
#6955=EDGE_CURVE('',#5663,#5663,#4761,.T.);
#6956=EDGE_CURVE('',#5663,#5664,#3282,.T.);
#6957=EDGE_CURVE('',#5664,#5664,#4762,.T.);
#6958=EDGE_CURVE('',#5665,#5665,#4763,.T.);
#6959=EDGE_CURVE('',#5665,#5662,#3283,.T.);
#6960=EDGE_CURVE('',#5666,#5667,#3284,.T.);
#6961=EDGE_CURVE('',#5668,#5666,#4764,.T.);
#6962=EDGE_CURVE('',#5669,#5668,#3285,.T.);
#6963=EDGE_CURVE('',#5667,#5669,#4765,.T.);
#6964=EDGE_CURVE('',#5670,#5671,#3286,.T.);
#6965=EDGE_CURVE('',#5672,#5670,#4766,.T.);
#6966=EDGE_CURVE('',#5673,#5672,#3287,.T.);
#6967=EDGE_CURVE('',#5671,#5673,#4767,.T.);
#6968=EDGE_CURVE('',#5674,#5675,#3288,.T.);
#6969=EDGE_CURVE('',#5676,#5674,#4768,.T.);
#6970=EDGE_CURVE('',#5677,#5676,#3289,.T.);
#6971=EDGE_CURVE('',#5675,#5677,#4769,.T.);
#6972=EDGE_CURVE('',#5678,#5679,#3290,.T.);
#6973=EDGE_CURVE('',#5680,#5678,#4770,.T.);
#6974=EDGE_CURVE('',#5681,#5680,#3291,.T.);
#6975=EDGE_CURVE('',#5679,#5681,#4771,.T.);
#6976=EDGE_CURVE('',#5680,#5666,#4772,.T.);
#6977=EDGE_CURVE('',#5676,#5678,#4773,.T.);
#6978=EDGE_CURVE('',#5672,#5674,#4774,.T.);
#6979=EDGE_CURVE('',#5668,#5670,#4775,.T.);
#6980=EDGE_CURVE('',#5682,#5682,#4776,.T.);
#6981=EDGE_CURVE('',#5677,#5679,#4777,.T.);
#6982=EDGE_CURVE('',#5673,#5675,#4778,.T.);
#6983=EDGE_CURVE('',#5681,#5667,#4779,.T.);
#6984=EDGE_CURVE('',#5669,#5671,#4780,.T.);
#6985=EDGE_CURVE('',#5682,#5683,#3292,.T.);
#6986=EDGE_CURVE('',#5683,#5683,#4781,.T.);
#6987=EDGE_CURVE('',#5684,#5684,#4782,.T.);
#6988=EDGE_CURVE('',#5685,#5685,#4783,.T.);
#6989=EDGE_CURVE('',#5685,#5684,#3293,.T.);
#6990=EDGE_CURVE('',#5686,#5686,#4784,.T.);
#6991=EDGE_CURVE('',#5686,#5687,#3294,.T.);
#6992=EDGE_CURVE('',#5687,#5687,#4785,.T.);
#6993=EDGE_CURVE('',#5688,#5688,#4786,.T.);
#6994=EDGE_CURVE('',#5688,#5689,#3295,.T.);
#6995=EDGE_CURVE('',#5689,#5689,#4787,.T.);
#6996=EDGE_CURVE('',#5690,#5690,#4788,.T.);
#6997=EDGE_CURVE('',#5690,#5691,#3296,.T.);
#6998=EDGE_CURVE('',#5691,#5691,#4789,.T.);
#6999=EDGE_CURVE('',#5692,#5693,#3297,.T.);
#7000=EDGE_CURVE('',#5693,#5694,#3298,.T.);
#7001=EDGE_CURVE('',#5695,#5694,#3299,.T.);
#7002=EDGE_CURVE('',#5692,#5695,#3300,.T.);
#7003=EDGE_CURVE('',#5696,#5692,#3301,.T.);
#7004=EDGE_CURVE('',#5697,#5695,#3302,.T.);
#7005=EDGE_CURVE('',#5696,#5697,#3303,.T.);
#7006=EDGE_CURVE('',#5698,#5696,#3304,.T.);
#7007=EDGE_CURVE('',#5699,#5697,#3305,.T.);
#7008=EDGE_CURVE('',#5698,#5699,#3306,.T.);
#7009=EDGE_CURVE('',#5693,#5698,#3307,.T.);
#7010=EDGE_CURVE('',#5694,#5699,#3308,.T.);
#7011=EDGE_CURVE('',#5700,#5700,#4790,.T.);
#7012=EDGE_CURVE('',#5700,#5701,#3309,.T.);
#7013=EDGE_CURVE('',#5701,#5701,#4791,.T.);
#7014=EDGE_CURVE('',#5702,#5703,#3310,.T.);
#7015=EDGE_CURVE('',#5702,#5703,#4792,.T.);
#7016=EDGE_CURVE('',#5704,#5705,#513,.T.);
#7017=EDGE_CURVE('',#5706,#5704,#4793,.T.);
#7018=EDGE_CURVE('',#5707,#5706,#514,.T.);
#7019=EDGE_CURVE('',#5703,#5707,#515,.T.);
#7020=EDGE_CURVE('',#5705,#5702,#516,.T.);
#7021=EDGE_CURVE('',#5705,#5708,#3311,.T.);
#7022=EDGE_CURVE('',#5708,#5708,#4794,.T.);
#7023=EDGE_CURVE('',#5706,#5704,#3312,.T.);
#7024=EDGE_CURVE('',#5709,#5709,#4795,.T.);
#7025=EDGE_CURVE('',#5709,#5705,#3313,.T.);
#7026=EDGE_CURVE('',#5707,#5710,#3314,.T.);
#7027=EDGE_CURVE('',#5710,#5710,#4796,.T.);
#7028=EDGE_CURVE('',#5711,#5712,#3315,.T.);
#7029=EDGE_CURVE('',#5712,#5713,#3316,.T.);
#7030=EDGE_CURVE('',#5714,#5713,#3317,.T.);
#7031=EDGE_CURVE('',#5711,#5714,#3318,.T.);
#7032=EDGE_CURVE('',#5715,#5711,#3319,.T.);
#7033=EDGE_CURVE('',#5716,#5714,#3320,.T.);
#7034=EDGE_CURVE('',#5715,#5716,#3321,.T.);
#7035=EDGE_CURVE('',#5717,#5715,#3322,.T.);
#7036=EDGE_CURVE('',#5718,#5716,#3323,.T.);
#7037=EDGE_CURVE('',#5717,#5718,#3324,.T.);
#7038=EDGE_CURVE('',#5712,#5717,#3325,.T.);
#7039=EDGE_CURVE('',#5713,#5718,#3326,.T.);
#7040=EDGE_CURVE('',#5719,#5720,#3327,.T.);
#7041=EDGE_CURVE('',#5719,#5720,#4797,.T.);
#7042=EDGE_CURVE('',#5721,#5719,#3328,.T.);
#7043=EDGE_CURVE('',#5722,#5721,#4798,.T.);
#7044=EDGE_CURVE('',#5722,#5723,#3329,.T.);
#7045=EDGE_CURVE('',#5723,#5723,#4799,.T.);
#7046=EDGE_CURVE('',#5724,#5722,#4800,.T.);
#7047=EDGE_CURVE('',#5720,#5724,#3330,.T.);
#7048=EDGE_CURVE('',#5725,#5726,#3331,.T.);
#7049=EDGE_CURVE('',#5725,#5726,#4801,.T.);
#7050=EDGE_CURVE('',#5727,#5725,#3332,.T.);
#7051=EDGE_CURVE('',#5728,#5727,#4802,.T.);
#7052=EDGE_CURVE('',#5728,#5729,#3333,.T.);
#7053=EDGE_CURVE('',#5729,#5729,#4803,.T.);
#7054=EDGE_CURVE('',#5730,#5728,#4804,.T.);
#7055=EDGE_CURVE('',#5726,#5730,#3334,.T.);
#7056=EDGE_CURVE('',#5731,#5732,#3335,.T.);
#7057=EDGE_CURVE('',#5731,#5732,#4805,.T.);
#7058=EDGE_CURVE('',#5733,#5731,#3336,.T.);
#7059=EDGE_CURVE('',#5734,#5733,#4806,.T.);
#7060=EDGE_CURVE('',#5734,#5735,#3337,.T.);
#7061=EDGE_CURVE('',#5735,#5735,#4807,.T.);
#7062=EDGE_CURVE('',#5736,#5734,#4808,.T.);
#7063=EDGE_CURVE('',#5732,#5736,#3338,.T.);
#7064=EDGE_CURVE('',#5737,#5738,#3339,.T.);
#7065=EDGE_CURVE('',#5737,#5738,#4809,.T.);
#7066=EDGE_CURVE('',#5739,#5737,#3340,.T.);
#7067=EDGE_CURVE('',#5740,#5739,#4810,.T.);
#7068=EDGE_CURVE('',#5740,#5741,#3341,.T.);
#7069=EDGE_CURVE('',#5741,#5741,#4811,.T.);
#7070=EDGE_CURVE('',#5742,#5740,#4812,.T.);
#7071=EDGE_CURVE('',#5738,#5742,#3342,.T.);
#7072=EDGE_CURVE('',#5724,#5733,#3343,.T.);
#7073=EDGE_CURVE('',#5736,#5743,#3344,.T.);
#7074=EDGE_CURVE('',#5744,#5743,#3345,.T.);
#7075=EDGE_CURVE('',#5744,#5745,#3346,.T.);
#7076=EDGE_CURVE('',#5746,#5745,#3347,.T.);
#7077=EDGE_CURVE('',#5746,#5721,#3348,.T.);
#7078=EDGE_CURVE('',#5730,#5739,#3349,.T.);
#7079=EDGE_CURVE('',#5742,#5747,#3350,.T.);
#7080=EDGE_CURVE('',#5748,#5747,#3351,.T.);
#7081=EDGE_CURVE('',#5749,#5748,#3352,.T.);
#7082=EDGE_CURVE('',#5750,#5749,#3353,.T.);
#7083=EDGE_CURVE('',#5750,#5727,#3354,.T.);
#7084=EDGE_CURVE('',#5743,#5751,#3355,.T.);
#7085=EDGE_CURVE('',#5751,#5752,#3356,.T.);
#7086=EDGE_CURVE('',#5752,#5753,#3357,.T.);
#7087=EDGE_CURVE('',#5753,#5754,#3358,.T.);
#7088=EDGE_CURVE('',#5754,#5750,#3359,.T.);
#7089=EDGE_CURVE('',#5749,#5755,#3360,.T.);
#7090=EDGE_CURVE('',#5755,#5756,#3361,.T.);
#7091=EDGE_CURVE('',#5756,#5757,#3362,.T.);
#7092=EDGE_CURVE('',#5757,#5758,#3363,.T.);
#7093=EDGE_CURVE('',#5758,#5744,#3364,.T.);
#7094=EDGE_CURVE('',#5759,#5746,#3365,.T.);
#7095=EDGE_CURVE('',#5751,#5759,#3366,.T.);
#7096=EDGE_CURVE('',#5760,#5759,#3367,.T.);
#7097=EDGE_CURVE('',#5752,#5760,#3368,.T.);
#7098=EDGE_CURVE('',#5761,#5760,#3369,.T.);
#7099=EDGE_CURVE('',#5753,#5761,#3370,.T.);
#7100=EDGE_CURVE('',#5762,#5761,#3371,.T.);
#7101=EDGE_CURVE('',#5754,#5762,#3372,.T.);
#7102=EDGE_CURVE('',#5747,#5762,#3373,.T.);
#7103=EDGE_CURVE('',#5763,#5748,#3374,.T.);
#7104=EDGE_CURVE('',#5755,#5763,#3375,.T.);
#7105=EDGE_CURVE('',#5764,#5763,#3376,.T.);
#7106=EDGE_CURVE('',#5756,#5764,#3377,.T.);
#7107=EDGE_CURVE('',#5765,#5764,#3378,.T.);
#7108=EDGE_CURVE('',#5757,#5765,#3379,.T.);
#7109=EDGE_CURVE('',#5766,#5765,#3380,.T.);
#7110=EDGE_CURVE('',#5758,#5766,#3381,.T.);
#7111=EDGE_CURVE('',#5745,#5766,#3382,.T.);
#7112=EDGE_CURVE('',#5767,#5768,#3383,.T.);
#7113=EDGE_CURVE('',#5768,#5769,#3384,.T.);
#7114=EDGE_CURVE('',#5770,#5769,#3385,.T.);
#7115=EDGE_CURVE('',#5767,#5770,#3386,.T.);
#7116=EDGE_CURVE('',#5771,#5767,#3387,.T.);
#7117=EDGE_CURVE('',#5772,#5770,#3388,.T.);
#7118=EDGE_CURVE('',#5771,#5772,#3389,.T.);
#7119=EDGE_CURVE('',#5773,#5771,#3390,.T.);
#7120=EDGE_CURVE('',#5774,#5772,#3391,.T.);
#7121=EDGE_CURVE('',#5773,#5774,#3392,.T.);
#7122=EDGE_CURVE('',#5775,#5773,#3393,.T.);
#7123=EDGE_CURVE('',#5776,#5774,#3394,.T.);
#7124=EDGE_CURVE('',#5775,#5776,#3395,.T.);
#7125=EDGE_CURVE('',#5777,#5775,#3396,.T.);
#7126=EDGE_CURVE('',#5778,#5776,#3397,.T.);
#7127=EDGE_CURVE('',#5777,#5778,#3398,.T.);
#7128=EDGE_CURVE('',#5779,#5777,#3399,.T.);
#7129=EDGE_CURVE('',#5780,#5778,#3400,.T.);
#7130=EDGE_CURVE('',#5779,#5780,#3401,.T.);
#7131=EDGE_CURVE('',#5781,#5779,#3402,.T.);
#7132=EDGE_CURVE('',#5782,#5780,#3403,.T.);
#7133=EDGE_CURVE('',#5781,#5782,#3404,.T.);
#7134=EDGE_CURVE('',#5768,#5781,#3405,.T.);
#7135=EDGE_CURVE('',#5769,#5782,#3406,.T.);
#7136=EDGE_CURVE('',#5783,#5784,#3407,.T.);
#7137=EDGE_CURVE('',#5783,#5785,#3408,.T.);
#7138=EDGE_CURVE('',#5786,#5785,#3409,.T.);
#7139=EDGE_CURVE('',#5784,#5786,#3410,.T.);
#7140=EDGE_CURVE('',#5784,#5787,#3411,.T.);
#7141=EDGE_CURVE('',#5788,#5786,#3412,.T.);
#7142=EDGE_CURVE('',#5787,#5788,#3413,.T.);
#7143=EDGE_CURVE('',#5787,#5789,#3414,.T.);
#7144=EDGE_CURVE('',#5790,#5788,#3415,.T.);
#7145=EDGE_CURVE('',#5789,#5790,#3416,.T.);
#7146=EDGE_CURVE('',#5789,#5791,#3417,.T.);
#7147=EDGE_CURVE('',#5792,#5790,#3418,.T.);
#7148=EDGE_CURVE('',#5791,#5792,#3419,.T.);
#7149=EDGE_CURVE('',#5791,#5793,#3420,.T.);
#7150=EDGE_CURVE('',#5794,#5792,#3421,.T.);
#7151=EDGE_CURVE('',#5793,#5794,#3422,.T.);
#7152=EDGE_CURVE('',#5793,#5795,#3423,.T.);
#7153=EDGE_CURVE('',#5796,#5794,#3424,.T.);
#7154=EDGE_CURVE('',#5795,#5796,#3425,.T.);
#7155=EDGE_CURVE('',#5795,#5797,#3426,.T.);
#7156=EDGE_CURVE('',#5798,#5796,#3427,.T.);
#7157=EDGE_CURVE('',#5797,#5798,#3428,.T.);
#7158=EDGE_CURVE('',#5797,#5783,#3429,.T.);
#7159=EDGE_CURVE('',#5785,#5798,#3430,.T.);
#7160=EDGE_CURVE('',#5799,#5800,#3431,.T.);
#7161=EDGE_CURVE('',#5800,#5801,#3432,.T.);
#7162=EDGE_CURVE('',#5801,#5802,#3433,.T.);
#7163=EDGE_CURVE('',#5799,#5802,#3434,.T.);
#7164=EDGE_CURVE('',#5800,#5803,#3435,.T.);
#7165=EDGE_CURVE('',#5803,#5804,#3436,.T.);
#7166=EDGE_CURVE('',#5804,#5801,#3437,.T.);
#7167=EDGE_CURVE('',#5803,#5805,#3438,.T.);
#7168=EDGE_CURVE('',#5805,#5806,#3439,.T.);
#7169=EDGE_CURVE('',#5806,#5804,#3440,.T.);
#7170=EDGE_CURVE('',#5805,#5807,#3441,.T.);
#7171=EDGE_CURVE('',#5807,#5808,#3442,.T.);
#7172=EDGE_CURVE('',#5808,#5806,#3443,.T.);
#7173=EDGE_CURVE('',#5807,#5809,#3444,.T.);
#7174=EDGE_CURVE('',#5809,#5810,#3445,.T.);
#7175=EDGE_CURVE('',#5810,#5808,#3446,.T.);
#7176=EDGE_CURVE('',#5809,#5799,#3447,.T.);
#7177=EDGE_CURVE('',#5802,#5810,#3448,.T.);
#7178=EDGE_CURVE('',#5811,#5811,#4813,.T.);
#7179=EDGE_CURVE('',#5812,#5812,#4814,.T.);
#7180=EDGE_CURVE('',#5813,#5813,#4815,.T.);
#7181=EDGE_CURVE('',#5813,#5812,#3449,.T.);
#7182=EDGE_CURVE('',#5814,#5814,#4816,.T.);
#7183=EDGE_CURVE('',#5814,#5813,#3450,.T.);
#7184=EDGE_CURVE('',#5815,#5815,#4817,.T.);
#7185=EDGE_CURVE('',#5815,#5814,#3451,.T.);
#7186=EDGE_CURVE('',#5816,#5816,#4818,.T.);
#7187=EDGE_CURVE('',#5817,#5817,#4819,.F.);
#7188=EDGE_CURVE('',#5817,#5816,#3452,.T.);
#7189=EDGE_CURVE('',#5811,#5817,#3453,.T.);
#7190=EDGE_CURVE('',#5818,#5819,#4820,.T.);
#7191=EDGE_CURVE('',#5819,#5818,#4821,.T.);
#7192=EDGE_CURVE('',#5819,#5820,#4822,.T.);
#7193=EDGE_CURVE('',#5821,#5820,#4823,.T.);
#7194=EDGE_CURVE('',#5820,#5821,#4824,.T.);
#7195=EDGE_CURVE('',#5821,#5822,#3454,.T.);
#7196=EDGE_CURVE('',#5822,#5822,#4825,.T.);
#7197=EDGE_CURVE('',#5823,#5823,#4826,.T.);
#7198=EDGE_CURVE('',#5823,#5824,#3455,.T.);
#7199=EDGE_CURVE('',#5824,#5824,#4827,.T.);
#7200=EDGE_CURVE('',#5824,#5825,#3456,.T.);
#7201=EDGE_CURVE('',#5825,#5825,#4828,.T.);
#7202=EDGE_CURVE('',#5826,#5826,#4829,.T.);
#7203=EDGE_CURVE('',#5826,#5818,#3457,.T.);
#7204=EDGE_CURVE('',#5827,#5827,#4830,.T.);
#7205=EDGE_CURVE('',#5827,#5823,#3458,.T.);
#7206=EDGE_CURVE('',#5828,#5829,#4831,.T.);
#7207=EDGE_CURVE('',#5829,#5828,#4832,.T.);
#7208=EDGE_CURVE('',#5829,#5830,#4833,.T.);
#7209=EDGE_CURVE('',#5831,#5830,#4834,.T.);
#7210=EDGE_CURVE('',#5830,#5831,#4835,.T.);
#7211=EDGE_CURVE('',#5832,#5832,#4836,.T.);
#7212=EDGE_CURVE('',#5832,#5831,#3459,.T.);
#7213=EDGE_CURVE('',#5833,#5833,#4837,.T.);
#7214=EDGE_CURVE('',#5834,#5834,#4838,.T.);
#7215=EDGE_CURVE('',#5835,#5835,#4839,.T.);
#7216=EDGE_CURVE('',#5835,#5833,#3460,.T.);
#7217=EDGE_CURVE('',#5836,#5836,#4840,.T.);
#7218=EDGE_CURVE('',#5836,#5835,#3461,.T.);
#7219=EDGE_CURVE('',#5837,#5837,#4841,.T.);
#7220=EDGE_CURVE('',#5837,#5836,#3462,.T.);
#7221=EDGE_CURVE('',#5828,#5834,#3463,.T.);
#7222=EDGE_CURVE('',#5838,#5839,#4842,.T.);
#7223=EDGE_CURVE('',#5840,#5841,#4843,.T.);
#7224=EDGE_CURVE('',#5842,#5843,#4844,.T.);
#7225=EDGE_CURVE('',#5844,#5845,#4845,.T.);
#7226=EDGE_CURVE('',#5846,#5847,#4846,.T.);
#7227=EDGE_CURVE('',#5848,#5849,#4847,.T.);
#7228=EDGE_CURVE('',#5850,#5851,#4848,.T.);
#7229=EDGE_CURVE('',#5852,#5853,#517,.T.);
#7230=EDGE_CURVE('',#5854,#5852,#4849,.T.);
#7231=EDGE_CURVE('',#5855,#5854,#518,.T.);
#7232=EDGE_CURVE('',#5853,#5855,#4850,.T.);
#7233=EDGE_CURVE('',#5856,#5854,#4851,.T.);
#7234=EDGE_CURVE('',#5856,#5857,#519,.T.);
#7235=EDGE_CURVE('',#5858,#5857,#4852,.T.);
#7236=EDGE_CURVE('',#5858,#5859,#520,.T.);
#7237=EDGE_CURVE('',#5860,#5859,#4853,.T.);
#7238=EDGE_CURVE('',#5860,#5861,#3464,.T.);
#7239=EDGE_CURVE('',#5861,#5861,#4854,.T.);
#7240=EDGE_CURVE('',#5862,#5860,#4855,.T.);
#7241=EDGE_CURVE('',#5862,#5863,#521,.T.);
#7242=EDGE_CURVE('',#5864,#5863,#4856,.T.);
#7243=EDGE_CURVE('',#5864,#5865,#522,.T.);
#7244=EDGE_CURVE('',#5866,#5865,#4857,.T.);
#7245=EDGE_CURVE('',#5866,#5867,#523,.T.);
#7246=EDGE_CURVE('',#5868,#5867,#4858,.T.);
#7247=EDGE_CURVE('',#5868,#5869,#524,.T.);
#7248=EDGE_CURVE('',#5855,#5869,#4859,.T.);
#7249=EDGE_CURVE('',#5852,#5870,#4860,.T.);
#7250=EDGE_CURVE('',#5870,#5856,#4861,.T.);
#7251=EDGE_CURVE('',#5871,#5870,#525,.T.);
#7252=EDGE_CURVE('',#5857,#5871,#4862,.T.);
#7253=EDGE_CURVE('',#5871,#5872,#4863,.T.);
#7254=EDGE_CURVE('',#5872,#5858,#4864,.T.);
#7255=EDGE_CURVE('',#5873,#5872,#526,.T.);
#7256=EDGE_CURVE('',#5859,#5873,#4865,.T.);
#7257=EDGE_CURVE('',#5873,#5874,#4866,.T.);
#7258=EDGE_CURVE('',#5874,#5875,#4867,.T.);
#7259=EDGE_CURVE('',#5875,#5862,#4868,.T.);
#7260=EDGE_CURVE('',#5876,#5875,#527,.T.);
#7261=EDGE_CURVE('',#5863,#5876,#4869,.T.);
#7262=EDGE_CURVE('',#5876,#5877,#4870,.T.);
#7263=EDGE_CURVE('',#5877,#5864,#4871,.T.);
#7264=EDGE_CURVE('',#5878,#5877,#528,.T.);
#7265=EDGE_CURVE('',#5865,#5878,#4872,.T.);
#7266=EDGE_CURVE('',#5878,#5879,#4873,.T.);
#7267=EDGE_CURVE('',#5879,#5866,#4874,.T.);
#7268=EDGE_CURVE('',#5880,#5879,#529,.T.);
#7269=EDGE_CURVE('',#5867,#5880,#4875,.T.);
#7270=EDGE_CURVE('',#5881,#5881,#4876,.T.);
#7271=EDGE_CURVE('',#5881,#5874,#3465,.T.);
#7272=EDGE_CURVE('',#5882,#5853,#4877,.T.);
#7273=EDGE_CURVE('',#5882,#5883,#530,.T.);
#7274=EDGE_CURVE('',#5880,#5883,#4878,.T.);
#7275=EDGE_CURVE('',#5869,#5882,#4879,.T.);
#7276=EDGE_CURVE('',#5883,#5868,#4880,.T.);
#7277=EDGE_CURVE('',#5884,#5884,#4881,.T.);
#7278=EDGE_CURVE('',#5885,#5885,#4882,.T.);
#7279=EDGE_CURVE('',#5886,#5886,#4883,.T.);
#7280=EDGE_CURVE('',#5886,#5884,#3466,.T.);
#7281=EDGE_CURVE('',#5887,#5887,#4884,.T.);
#7282=EDGE_CURVE('',#5887,#5885,#3467,.T.);
#7283=EDGE_CURVE('',#5888,#5888,#4885,.T.);
#7284=EDGE_CURVE('',#5889,#5889,#4886,.T.);
#7285=EDGE_CURVE('',#5890,#5890,#4887,.T.);
#7286=EDGE_CURVE('',#5890,#5888,#3468,.T.);
#7287=EDGE_CURVE('',#5891,#5891,#4888,.T.);
#7288=EDGE_CURVE('',#5891,#5889,#3469,.T.);
#7289=EDGE_CURVE('',#5892,#5893,#3470,.T.);
#7290=EDGE_CURVE('',#5893,#5894,#3471,.T.);
#7291=EDGE_CURVE('',#5894,#5895,#3472,.T.);
#7292=EDGE_CURVE('',#5892,#5895,#3473,.T.);
#7293=EDGE_CURVE('',#5893,#5896,#3474,.T.);
#7294=EDGE_CURVE('',#5896,#5897,#3475,.T.);
#7295=EDGE_CURVE('',#5897,#5894,#3476,.T.);
#7296=EDGE_CURVE('',#5896,#5898,#3477,.T.);
#7297=EDGE_CURVE('',#5898,#5899,#3478,.T.);
#7298=EDGE_CURVE('',#5899,#5897,#3479,.T.);
#7299=EDGE_CURVE('',#5898,#5900,#3480,.T.);
#7300=EDGE_CURVE('',#5900,#5901,#3481,.T.);
#7301=EDGE_CURVE('',#5901,#5899,#3482,.T.);
#7302=EDGE_CURVE('',#5900,#5902,#3483,.T.);
#7303=EDGE_CURVE('',#5902,#5903,#3484,.T.);
#7304=EDGE_CURVE('',#5903,#5901,#3485,.T.);
#7305=EDGE_CURVE('',#5902,#5892,#3486,.T.);
#7306=EDGE_CURVE('',#5895,#5903,#3487,.T.);
#7307=EDGE_CURVE('',#5904,#5904,#4889,.T.);
#7308=EDGE_CURVE('',#5905,#5905,#4890,.T.);
#7309=EDGE_CURVE('',#5906,#5906,#4891,.T.);
#7310=EDGE_CURVE('',#5906,#5905,#3488,.T.);
#7311=EDGE_CURVE('',#5907,#5907,#4892,.T.);
#7312=EDGE_CURVE('',#5907,#5906,#3489,.T.);
#7313=EDGE_CURVE('',#5908,#5908,#4893,.T.);
#7314=EDGE_CURVE('',#5908,#5907,#3490,.T.);
#7315=EDGE_CURVE('',#5909,#5909,#4894,.T.);
#7316=EDGE_CURVE('',#5910,#5910,#4895,.F.);
#7317=EDGE_CURVE('',#5910,#5909,#3491,.T.);
#7318=EDGE_CURVE('',#5904,#5910,#3492,.T.);
#7319=EDGE_CURVE('',#5911,#5911,#4896,.T.);
#7320=EDGE_CURVE('',#5911,#5912,#3493,.T.);
#7321=EDGE_CURVE('',#5912,#5912,#4897,.T.);
#7322=EDGE_CURVE('',#5913,#5913,#4898,.T.);
#7323=EDGE_CURVE('',#5914,#5914,#4899,.T.);
#7324=EDGE_CURVE('',#5915,#5915,#4900,.T.);
#7325=EDGE_CURVE('',#5916,#5916,#4901,.T.);
#7326=EDGE_CURVE('',#5913,#5915,#3494,.T.);
#7327=EDGE_CURVE('',#5916,#5917,#3495,.T.);
#7328=EDGE_CURVE('',#5917,#5917,#4902,.T.);
#7329=EDGE_CURVE('',#5918,#5918,#4903,.T.);
#7330=EDGE_CURVE('',#5918,#5919,#3496,.T.);
#7331=EDGE_CURVE('',#5919,#5919,#4904,.T.);
#7332=EDGE_CURVE('',#5920,#5920,#4905,.T.);
#7333=EDGE_CURVE('',#5920,#5914,#3497,.T.);
#7334=EDGE_CURVE('',#5921,#5921,#4906,.T.);
#7335=EDGE_CURVE('',#5921,#5922,#3498,.T.);
#7336=EDGE_CURVE('',#5922,#5922,#4907,.T.);
#7337=EDGE_CURVE('',#5923,#5923,#4908,.T.);
#7338=EDGE_CURVE('',#5923,#5924,#3499,.T.);
#7339=EDGE_CURVE('',#5924,#5924,#4909,.T.);
#7340=EDGE_CURVE('',#5925,#5925,#4910,.T.);
#7341=EDGE_CURVE('',#5925,#5926,#3500,.T.);
#7342=EDGE_CURVE('',#5926,#5926,#4911,.T.);
#7343=EDGE_CURVE('',#5927,#5927,#4912,.T.);
#7344=EDGE_CURVE('',#5927,#5928,#3501,.T.);
#7345=EDGE_CURVE('',#5928,#5928,#4913,.T.);
#7346=EDGE_CURVE('',#5929,#5929,#4914,.T.);
#7347=EDGE_CURVE('',#5929,#5930,#3502,.T.);
#7348=EDGE_CURVE('',#5930,#5930,#4915,.T.);
#7349=EDGE_CURVE('',#5931,#5931,#4916,.T.);
#7350=EDGE_CURVE('',#5931,#5932,#3503,.T.);
#7351=EDGE_CURVE('',#5932,#5932,#4917,.T.);
#7352=EDGE_CURVE('',#5933,#5933,#4918,.T.);
#7353=EDGE_CURVE('',#5933,#5934,#3504,.T.);
#7354=EDGE_CURVE('',#5934,#5934,#4919,.T.);
#7355=EDGE_CURVE('',#5935,#5935,#4920,.T.);
#7356=EDGE_CURVE('',#5935,#5936,#3505,.T.);
#7357=EDGE_CURVE('',#5936,#5936,#4921,.T.);
#7358=EDGE_CURVE('',#5937,#5937,#4922,.T.);
#7359=EDGE_CURVE('',#5937,#5938,#3506,.T.);
#7360=EDGE_CURVE('',#5938,#5938,#4923,.T.);
#7361=EDGE_CURVE('',#5939,#5940,#531,.T.);
#7362=EDGE_CURVE('',#5941,#5939,#532,.T.);
#7363=EDGE_CURVE('',#5940,#5941,#533,.T.);
#7364=EDGE_CURVE('',#5940,#5942,#3507,.T.);
#7365=EDGE_CURVE('',#5943,#5942,#534,.T.);
#7366=EDGE_CURVE('',#5944,#5943,#535,.T.);
#7367=EDGE_CURVE('',#5945,#5944,#536,.T.);
#7368=EDGE_CURVE('',#5942,#5945,#537,.T.);
#7369=EDGE_CURVE('',#5946,#5947,#538,.T.);
#7370=EDGE_CURVE('',#5947,#5946,#539,.T.);
#7371=EDGE_CURVE('',#5947,#5948,#3508,.T.);
#7372=EDGE_CURVE('',#5949,#5948,#540,.T.);
#7373=EDGE_CURVE('',#5950,#5949,#541,.T.);
#7374=EDGE_CURVE('',#5948,#5950,#542,.T.);
#7375=EDGE_CURVE('',#5951,#5951,#4924,.T.);
#7376=EDGE_CURVE('',#5951,#5941,#3509,.T.);
#7377=EDGE_CURVE('',#5939,#5952,#3510,.T.);
#7378=EDGE_CURVE('',#5952,#5952,#4925,.T.);
#7379=EDGE_CURVE('',#5953,#5954,#543,.T.);
#7380=EDGE_CURVE('',#5954,#5955,#544,.T.);
#7381=EDGE_CURVE('',#5955,#5953,#545,.T.);
#7382=EDGE_CURVE('',#5956,#5957,#546,.T.);
#7383=EDGE_CURVE('',#5957,#5958,#547,.T.);
#7384=EDGE_CURVE('',#5958,#5956,#548,.T.);
#7385=EDGE_CURVE('',#5955,#5959,#3511,.T.);
#7386=EDGE_CURVE('',#5960,#5959,#549,.T.);
#7387=EDGE_CURVE('',#5959,#5960,#550,.T.);
#7388=EDGE_CURVE('',#5961,#5962,#551,.T.);
#7389=EDGE_CURVE('',#5962,#5961,#552,.T.);
#7390=EDGE_CURVE('',#5962,#5958,#3512,.T.);
#7391=EDGE_CURVE('',#5963,#5963,#4926,.T.);
#7392=EDGE_CURVE('',#5963,#5943,#3513,.T.);
#7393=EDGE_CURVE('',#5945,#5964,#3514,.T.);
#7394=EDGE_CURVE('',#5964,#5964,#4927,.T.);
#7395=EDGE_CURVE('',#5965,#5965,#4928,.T.);
#7396=EDGE_CURVE('',#5966,#5967,#4929,.T.);
#7397=EDGE_CURVE('',#5968,#5967,#4930,.T.);
#7398=EDGE_CURVE('',#5968,#5969,#4931,.T.);
#7399=EDGE_CURVE('',#5970,#5969,#4932,.T.);
#7400=EDGE_CURVE('',#5970,#5971,#4933,.T.);
#7401=EDGE_CURVE('',#5972,#5971,#4934,.T.);
#7402=EDGE_CURVE('',#5972,#5973,#4935,.T.);
#7403=EDGE_CURVE('',#5974,#5973,#4936,.T.);
#7404=EDGE_CURVE('',#5974,#5975,#4937,.T.);
#7405=EDGE_CURVE('',#5976,#5975,#4938,.T.);
#7406=EDGE_CURVE('',#5976,#5977,#4939,.T.);
#7407=EDGE_CURVE('',#5978,#5977,#4940,.T.);
#7408=EDGE_CURVE('',#5978,#5979,#4941,.T.);
#7409=EDGE_CURVE('',#5980,#5979,#4942,.T.);
#7410=EDGE_CURVE('',#5980,#5981,#4943,.T.);
#7411=EDGE_CURVE('',#5982,#5981,#4944,.T.);
#7412=EDGE_CURVE('',#5982,#5983,#4945,.T.);
#7413=EDGE_CURVE('',#5984,#5983,#4946,.T.);
#7414=EDGE_CURVE('',#5984,#5985,#4947,.T.);
#7415=EDGE_CURVE('',#5986,#5985,#4948,.T.);
#7416=EDGE_CURVE('',#5986,#5987,#4949,.T.);
#7417=EDGE_CURVE('',#5988,#5987,#4950,.T.);
#7418=EDGE_CURVE('',#5988,#5989,#4951,.T.);
#7419=EDGE_CURVE('',#5990,#5989,#4952,.T.);
#7420=EDGE_CURVE('',#5990,#5991,#4953,.T.);
#7421=EDGE_CURVE('',#5992,#5991,#4954,.T.);
#7422=EDGE_CURVE('',#5992,#5993,#4955,.T.);
#7423=EDGE_CURVE('',#5994,#5993,#4956,.T.);
#7424=EDGE_CURVE('',#5994,#5995,#4957,.T.);
#7425=EDGE_CURVE('',#5996,#5995,#4958,.T.);
#7426=EDGE_CURVE('',#5996,#5997,#4959,.T.);
#7427=EDGE_CURVE('',#5998,#5997,#4960,.T.);
#7428=EDGE_CURVE('',#5998,#5999,#4961,.T.);
#7429=EDGE_CURVE('',#6000,#5999,#4962,.T.);
#7430=EDGE_CURVE('',#6000,#6001,#4963,.T.);
#7431=EDGE_CURVE('',#6002,#6001,#4964,.T.);
#7432=EDGE_CURVE('',#6002,#6003,#4965,.T.);
#7433=EDGE_CURVE('',#6004,#6003,#4966,.T.);
#7434=EDGE_CURVE('',#6004,#6005,#4967,.T.);
#7435=EDGE_CURVE('',#5966,#6005,#4968,.T.);
#7436=EDGE_CURVE('',#6006,#6006,#4969,.T.);
#7437=EDGE_CURVE('',#6006,#5965,#3515,.T.);
#7438=EDGE_CURVE('',#6007,#6007,#4970,.T.);
#7439=EDGE_CURVE('',#6008,#6009,#4971,.T.);
#7440=EDGE_CURVE('',#6009,#6010,#4972,.T.);
#7441=EDGE_CURVE('',#6010,#6011,#4973,.T.);
#7442=EDGE_CURVE('',#6011,#6012,#4974,.T.);
#7443=EDGE_CURVE('',#6012,#6013,#4975,.T.);
#7444=EDGE_CURVE('',#6013,#6014,#4976,.T.);
#7445=EDGE_CURVE('',#6014,#6015,#4977,.T.);
#7446=EDGE_CURVE('',#6015,#6016,#4978,.T.);
#7447=EDGE_CURVE('',#6016,#6017,#4979,.T.);
#7448=EDGE_CURVE('',#6017,#6018,#4980,.T.);
#7449=EDGE_CURVE('',#6018,#6019,#4981,.T.);
#7450=EDGE_CURVE('',#6019,#6020,#4982,.T.);
#7451=EDGE_CURVE('',#6020,#6021,#4983,.T.);
#7452=EDGE_CURVE('',#6021,#6022,#4984,.T.);
#7453=EDGE_CURVE('',#6022,#6023,#4985,.T.);
#7454=EDGE_CURVE('',#6023,#6024,#4986,.T.);
#7455=EDGE_CURVE('',#6024,#6025,#4987,.T.);
#7456=EDGE_CURVE('',#6025,#6026,#4988,.T.);
#7457=EDGE_CURVE('',#6026,#6027,#4989,.T.);
#7458=EDGE_CURVE('',#6027,#6028,#4990,.T.);
#7459=EDGE_CURVE('',#6028,#6029,#4991,.T.);
#7460=EDGE_CURVE('',#6029,#6030,#4992,.T.);
#7461=EDGE_CURVE('',#6030,#6031,#4993,.T.);
#7462=EDGE_CURVE('',#6031,#6032,#4994,.T.);
#7463=EDGE_CURVE('',#6032,#6033,#4995,.T.);
#7464=EDGE_CURVE('',#6033,#6034,#4996,.T.);
#7465=EDGE_CURVE('',#6034,#6035,#4997,.T.);
#7466=EDGE_CURVE('',#6035,#6036,#4998,.T.);
#7467=EDGE_CURVE('',#6036,#6037,#4999,.T.);
#7468=EDGE_CURVE('',#6037,#6038,#5000,.T.);
#7469=EDGE_CURVE('',#6038,#6039,#5001,.T.);
#7470=EDGE_CURVE('',#6039,#6040,#5002,.T.);
#7471=EDGE_CURVE('',#6040,#6041,#5003,.T.);
#7472=EDGE_CURVE('',#6041,#6042,#5004,.T.);
#7473=EDGE_CURVE('',#6042,#6043,#5005,.T.);
#7474=EDGE_CURVE('',#6043,#6044,#5006,.T.);
#7475=EDGE_CURVE('',#6044,#6045,#5007,.T.);
#7476=EDGE_CURVE('',#6045,#6046,#5008,.T.);
#7477=EDGE_CURVE('',#6046,#6047,#5009,.T.);
#7478=EDGE_CURVE('',#6047,#6008,#5010,.T.);
#7479=EDGE_CURVE('',#6048,#6048,#5011,.T.);
#7480=EDGE_CURVE('',#6048,#6007,#3516,.T.);
#7481=EDGE_CURVE('',#6009,#5966,#3517,.T.);
#7482=EDGE_CURVE('',#5967,#6008,#3518,.T.);
#7483=EDGE_CURVE('',#6047,#5968,#3519,.T.);
#7484=EDGE_CURVE('',#5969,#6046,#3520,.T.);
#7485=EDGE_CURVE('',#6045,#5970,#3521,.T.);
#7486=EDGE_CURVE('',#5971,#6044,#3522,.T.);
#7487=EDGE_CURVE('',#6043,#5972,#3523,.T.);
#7488=EDGE_CURVE('',#5973,#6042,#3524,.T.);
#7489=EDGE_CURVE('',#6041,#5974,#3525,.T.);
#7490=EDGE_CURVE('',#5975,#6040,#3526,.T.);
#7491=EDGE_CURVE('',#6039,#5976,#3527,.T.);
#7492=EDGE_CURVE('',#5977,#6038,#3528,.T.);
#7493=EDGE_CURVE('',#6037,#5978,#3529,.T.);
#7494=EDGE_CURVE('',#5979,#6036,#3530,.T.);
#7495=EDGE_CURVE('',#6035,#5980,#3531,.T.);
#7496=EDGE_CURVE('',#5981,#6034,#3532,.T.);
#7497=EDGE_CURVE('',#6033,#5982,#3533,.T.);
#7498=EDGE_CURVE('',#5983,#6032,#3534,.T.);
#7499=EDGE_CURVE('',#6031,#5984,#3535,.T.);
#7500=EDGE_CURVE('',#5985,#6030,#3536,.T.);
#7501=EDGE_CURVE('',#6029,#5986,#3537,.T.);
#7502=EDGE_CURVE('',#5987,#6028,#3538,.T.);
#7503=EDGE_CURVE('',#6027,#5988,#3539,.T.);
#7504=EDGE_CURVE('',#5989,#6026,#3540,.T.);
#7505=EDGE_CURVE('',#6025,#5990,#3541,.T.);
#7506=EDGE_CURVE('',#5991,#6024,#3542,.T.);
#7507=EDGE_CURVE('',#6023,#5992,#3543,.T.);
#7508=EDGE_CURVE('',#5993,#6022,#3544,.T.);
#7509=EDGE_CURVE('',#6021,#5994,#3545,.T.);
#7510=EDGE_CURVE('',#5995,#6020,#3546,.T.);
#7511=EDGE_CURVE('',#6019,#5996,#3547,.T.);
#7512=EDGE_CURVE('',#5997,#6018,#3548,.T.);
#7513=EDGE_CURVE('',#6017,#5998,#3549,.T.);
#7514=EDGE_CURVE('',#5999,#6016,#3550,.T.);
#7515=EDGE_CURVE('',#6015,#6000,#3551,.T.);
#7516=EDGE_CURVE('',#6001,#6014,#3552,.T.);
#7517=EDGE_CURVE('',#6013,#6002,#3553,.T.);
#7518=EDGE_CURVE('',#6003,#6012,#3554,.T.);
#7519=EDGE_CURVE('',#6005,#6010,#3555,.T.);
#7520=EDGE_CURVE('',#6011,#6004,#3556,.T.);
#7521=EDGE_CURVE('',#6049,#6049,#5012,.T.);
#7522=EDGE_CURVE('',#6049,#6050,#3557,.T.);
#7523=EDGE_CURVE('',#6050,#6050,#5013,.T.);
#7524=EDGE_CURVE('',#6051,#6051,#5014,.T.);
#7525=EDGE_CURVE('',#6052,#6052,#5015,.T.);
#7526=EDGE_CURVE('',#6053,#6053,#5016,.T.);
#7527=EDGE_CURVE('',#6054,#6054,#5017,.T.);
#7528=EDGE_CURVE('',#6051,#6053,#3558,.T.);
#7529=EDGE_CURVE('',#6054,#6055,#3559,.T.);
#7530=EDGE_CURVE('',#6055,#6055,#5018,.T.);
#7531=EDGE_CURVE('',#6056,#6056,#5019,.T.);
#7532=EDGE_CURVE('',#6056,#6052,#3560,.T.);
#7533=EDGE_CURVE('',#6057,#6057,#5020,.T.);
#7534=EDGE_CURVE('',#6057,#6058,#3561,.T.);
#7535=EDGE_CURVE('',#6058,#6058,#5021,.T.);
#7536=EDGE_CURVE('',#6059,#6059,#5022,.T.);
#7537=EDGE_CURVE('',#6059,#6060,#3562,.T.);
#7538=EDGE_CURVE('',#6060,#6060,#5023,.T.);
#7539=EDGE_CURVE('',#6061,#6061,#5024,.T.);
#7540=EDGE_CURVE('',#6061,#6062,#3563,.T.);
#7541=EDGE_CURVE('',#6062,#6062,#5025,.T.);
#7542=EDGE_CURVE('',#6063,#6063,#5026,.T.);
#7543=EDGE_CURVE('',#6063,#6064,#3564,.T.);
#7544=EDGE_CURVE('',#6064,#6064,#5027,.T.);
#7545=EDGE_CURVE('',#6065,#6065,#5028,.T.);
#7546=EDGE_CURVE('',#6065,#6066,#3565,.T.);
#7547=EDGE_CURVE('',#6066,#6066,#5029,.T.);
#7548=EDGE_CURVE('',#6067,#6067,#5030,.T.);
#7549=EDGE_CURVE('',#6067,#6068,#3566,.T.);
#7550=EDGE_CURVE('',#6068,#6068,#5031,.T.);
#7551=EDGE_CURVE('',#6069,#6069,#5032,.T.);
#7552=EDGE_CURVE('',#6069,#6070,#3567,.T.);
#7553=EDGE_CURVE('',#6070,#6070,#5033,.T.);
#7554=EDGE_CURVE('',#6071,#6071,#5034,.T.);
#7555=EDGE_CURVE('',#6071,#6072,#3568,.T.);
#7556=EDGE_CURVE('',#6072,#6072,#5035,.T.);
#7557=EDGE_CURVE('',#6073,#6074,#553,.T.);
#7558=EDGE_CURVE('',#6075,#6073,#554,.T.);
#7559=EDGE_CURVE('',#6074,#6075,#555,.T.);
#7560=EDGE_CURVE('',#6074,#6076,#3569,.T.);
#7561=EDGE_CURVE('',#6077,#6076,#556,.T.);
#7562=EDGE_CURVE('',#6078,#6077,#557,.T.);
#7563=EDGE_CURVE('',#6079,#6078,#558,.T.);
#7564=EDGE_CURVE('',#6076,#6079,#559,.T.);
#7565=EDGE_CURVE('',#6080,#6081,#560,.T.);
#7566=EDGE_CURVE('',#6081,#6080,#561,.T.);
#7567=EDGE_CURVE('',#6081,#6082,#3570,.T.);
#7568=EDGE_CURVE('',#6083,#6082,#562,.T.);
#7569=EDGE_CURVE('',#6084,#6083,#563,.T.);
#7570=EDGE_CURVE('',#6082,#6084,#564,.T.);
#7571=EDGE_CURVE('',#6085,#6085,#5036,.T.);
#7572=EDGE_CURVE('',#6085,#6075,#3571,.T.);
#7573=EDGE_CURVE('',#6073,#6086,#3572,.T.);
#7574=EDGE_CURVE('',#6086,#6086,#5037,.T.);
#7575=EDGE_CURVE('',#6087,#6088,#565,.T.);
#7576=EDGE_CURVE('',#6088,#6089,#566,.T.);
#7577=EDGE_CURVE('',#6089,#6087,#567,.T.);
#7578=EDGE_CURVE('',#6090,#6091,#568,.T.);
#7579=EDGE_CURVE('',#6091,#6092,#569,.T.);
#7580=EDGE_CURVE('',#6092,#6090,#570,.T.);
#7581=EDGE_CURVE('',#6089,#6093,#3573,.T.);
#7582=EDGE_CURVE('',#6094,#6093,#571,.T.);
#7583=EDGE_CURVE('',#6093,#6094,#572,.T.);
#7584=EDGE_CURVE('',#6095,#6096,#573,.T.);
#7585=EDGE_CURVE('',#6096,#6095,#574,.T.);
#7586=EDGE_CURVE('',#6096,#6092,#3574,.T.);
#7587=EDGE_CURVE('',#6097,#6097,#5038,.T.);
#7588=EDGE_CURVE('',#6097,#6077,#3575,.T.);
#7589=EDGE_CURVE('',#6079,#6098,#3576,.T.);
#7590=EDGE_CURVE('',#6098,#6098,#5039,.T.);
#7591=EDGE_CURVE('',#6099,#6099,#5040,.T.);
#7592=EDGE_CURVE('',#6100,#6101,#5041,.T.);
#7593=EDGE_CURVE('',#6102,#6101,#5042,.T.);
#7594=EDGE_CURVE('',#6102,#6103,#5043,.T.);
#7595=EDGE_CURVE('',#6104,#6103,#5044,.T.);
#7596=EDGE_CURVE('',#6104,#6105,#5045,.T.);
#7597=EDGE_CURVE('',#6106,#6105,#5046,.T.);
#7598=EDGE_CURVE('',#6106,#6107,#5047,.T.);
#7599=EDGE_CURVE('',#6108,#6107,#5048,.T.);
#7600=EDGE_CURVE('',#6108,#6109,#5049,.T.);
#7601=EDGE_CURVE('',#6110,#6109,#5050,.T.);
#7602=EDGE_CURVE('',#6110,#6111,#5051,.T.);
#7603=EDGE_CURVE('',#6112,#6111,#5052,.T.);
#7604=EDGE_CURVE('',#6112,#6113,#5053,.T.);
#7605=EDGE_CURVE('',#6114,#6113,#5054,.T.);
#7606=EDGE_CURVE('',#6114,#6115,#5055,.T.);
#7607=EDGE_CURVE('',#6116,#6115,#5056,.T.);
#7608=EDGE_CURVE('',#6116,#6117,#5057,.T.);
#7609=EDGE_CURVE('',#6118,#6117,#5058,.T.);
#7610=EDGE_CURVE('',#6118,#6119,#5059,.T.);
#7611=EDGE_CURVE('',#6120,#6119,#5060,.T.);
#7612=EDGE_CURVE('',#6120,#6121,#5061,.T.);
#7613=EDGE_CURVE('',#6122,#6121,#5062,.T.);
#7614=EDGE_CURVE('',#6122,#6123,#5063,.T.);
#7615=EDGE_CURVE('',#6124,#6123,#5064,.T.);
#7616=EDGE_CURVE('',#6124,#6125,#5065,.T.);
#7617=EDGE_CURVE('',#6126,#6125,#5066,.T.);
#7618=EDGE_CURVE('',#6126,#6127,#5067,.T.);
#7619=EDGE_CURVE('',#6128,#6127,#5068,.T.);
#7620=EDGE_CURVE('',#6128,#6129,#5069,.T.);
#7621=EDGE_CURVE('',#6130,#6129,#5070,.T.);
#7622=EDGE_CURVE('',#6130,#6131,#5071,.T.);
#7623=EDGE_CURVE('',#6132,#6131,#5072,.T.);
#7624=EDGE_CURVE('',#6132,#6133,#5073,.T.);
#7625=EDGE_CURVE('',#6134,#6133,#5074,.T.);
#7626=EDGE_CURVE('',#6134,#6135,#5075,.T.);
#7627=EDGE_CURVE('',#6136,#6135,#5076,.T.);
#7628=EDGE_CURVE('',#6136,#6137,#5077,.T.);
#7629=EDGE_CURVE('',#6138,#6137,#5078,.T.);
#7630=EDGE_CURVE('',#6138,#6139,#5079,.T.);
#7631=EDGE_CURVE('',#6140,#6139,#5080,.T.);
#7632=EDGE_CURVE('',#6140,#6141,#5081,.T.);
#7633=EDGE_CURVE('',#6142,#6141,#5082,.T.);
#7634=EDGE_CURVE('',#6142,#6143,#5083,.T.);
#7635=EDGE_CURVE('',#6144,#6143,#5084,.T.);
#7636=EDGE_CURVE('',#6144,#6145,#5085,.T.);
#7637=EDGE_CURVE('',#6146,#6145,#5086,.T.);
#7638=EDGE_CURVE('',#6146,#6147,#5087,.T.);
#7639=EDGE_CURVE('',#6148,#6147,#5088,.T.);
#7640=EDGE_CURVE('',#6148,#6149,#5089,.T.);
#7641=EDGE_CURVE('',#6150,#6149,#5090,.T.);
#7642=EDGE_CURVE('',#6150,#6151,#5091,.T.);
#7643=EDGE_CURVE('',#6152,#6151,#5092,.T.);
#7644=EDGE_CURVE('',#6152,#6153,#5093,.T.);
#7645=EDGE_CURVE('',#6154,#6153,#5094,.T.);
#7646=EDGE_CURVE('',#6154,#6155,#5095,.T.);
#7647=EDGE_CURVE('',#6156,#6155,#5096,.T.);
#7648=EDGE_CURVE('',#6156,#6157,#5097,.T.);
#7649=EDGE_CURVE('',#6158,#6157,#5098,.T.);
#7650=EDGE_CURVE('',#6158,#6159,#5099,.T.);
#7651=EDGE_CURVE('',#6160,#6159,#5100,.T.);
#7652=EDGE_CURVE('',#6160,#6161,#5101,.T.);
#7653=EDGE_CURVE('',#6162,#6161,#5102,.T.);
#7654=EDGE_CURVE('',#6162,#6163,#5103,.T.);
#7655=EDGE_CURVE('',#6164,#6163,#5104,.T.);
#7656=EDGE_CURVE('',#6164,#6165,#5105,.T.);
#7657=EDGE_CURVE('',#6166,#6165,#5106,.T.);
#7658=EDGE_CURVE('',#6166,#6167,#5107,.T.);
#7659=EDGE_CURVE('',#6168,#6167,#5108,.T.);
#7660=EDGE_CURVE('',#6168,#6169,#5109,.T.);
#7661=EDGE_CURVE('',#6170,#6169,#5110,.T.);
#7662=EDGE_CURVE('',#6170,#6171,#5111,.T.);
#7663=EDGE_CURVE('',#6172,#6171,#5112,.T.);
#7664=EDGE_CURVE('',#6172,#6173,#5113,.T.);
#7665=EDGE_CURVE('',#6174,#6173,#5114,.T.);
#7666=EDGE_CURVE('',#6174,#6175,#5115,.T.);
#7667=EDGE_CURVE('',#6176,#6175,#5116,.T.);
#7668=EDGE_CURVE('',#6176,#6177,#5117,.T.);
#7669=EDGE_CURVE('',#6178,#6177,#5118,.T.);
#7670=EDGE_CURVE('',#6178,#6179,#5119,.T.);
#7671=EDGE_CURVE('',#6100,#6179,#5120,.T.);
#7672=EDGE_CURVE('',#6180,#6180,#5121,.T.);
#7673=EDGE_CURVE('',#6180,#6099,#3577,.T.);
#7674=EDGE_CURVE('',#6181,#6181,#5122,.T.);
#7675=EDGE_CURVE('',#6182,#6183,#5123,.T.);
#7676=EDGE_CURVE('',#6183,#6184,#5124,.T.);
#7677=EDGE_CURVE('',#6184,#6185,#5125,.T.);
#7678=EDGE_CURVE('',#6185,#6186,#5126,.T.);
#7679=EDGE_CURVE('',#6186,#6187,#5127,.T.);
#7680=EDGE_CURVE('',#6187,#6188,#5128,.T.);
#7681=EDGE_CURVE('',#6188,#6189,#5129,.T.);
#7682=EDGE_CURVE('',#6189,#6190,#5130,.T.);
#7683=EDGE_CURVE('',#6190,#6191,#5131,.T.);
#7684=EDGE_CURVE('',#6191,#6192,#5132,.T.);
#7685=EDGE_CURVE('',#6192,#6193,#5133,.T.);
#7686=EDGE_CURVE('',#6193,#6194,#5134,.T.);
#7687=EDGE_CURVE('',#6194,#6195,#5135,.T.);
#7688=EDGE_CURVE('',#6195,#6196,#5136,.T.);
#7689=EDGE_CURVE('',#6196,#6197,#5137,.T.);
#7690=EDGE_CURVE('',#6197,#6198,#5138,.T.);
#7691=EDGE_CURVE('',#6198,#6199,#5139,.T.);
#7692=EDGE_CURVE('',#6199,#6200,#5140,.T.);
#7693=EDGE_CURVE('',#6200,#6201,#5141,.T.);
#7694=EDGE_CURVE('',#6201,#6202,#5142,.T.);
#7695=EDGE_CURVE('',#6202,#6203,#5143,.T.);
#7696=EDGE_CURVE('',#6203,#6204,#5144,.T.);
#7697=EDGE_CURVE('',#6204,#6205,#5145,.T.);
#7698=EDGE_CURVE('',#6205,#6206,#5146,.T.);
#7699=EDGE_CURVE('',#6206,#6207,#5147,.T.);
#7700=EDGE_CURVE('',#6207,#6208,#5148,.T.);
#7701=EDGE_CURVE('',#6208,#6209,#5149,.T.);
#7702=EDGE_CURVE('',#6209,#6210,#5150,.T.);
#7703=EDGE_CURVE('',#6210,#6211,#5151,.T.);
#7704=EDGE_CURVE('',#6211,#6212,#5152,.T.);
#7705=EDGE_CURVE('',#6212,#6213,#5153,.T.);
#7706=EDGE_CURVE('',#6213,#6214,#5154,.T.);
#7707=EDGE_CURVE('',#6214,#6215,#5155,.T.);
#7708=EDGE_CURVE('',#6215,#6216,#5156,.T.);
#7709=EDGE_CURVE('',#6216,#6217,#5157,.T.);
#7710=EDGE_CURVE('',#6217,#6218,#5158,.T.);
#7711=EDGE_CURVE('',#6218,#6219,#5159,.T.);
#7712=EDGE_CURVE('',#6219,#6220,#5160,.T.);
#7713=EDGE_CURVE('',#6220,#6221,#5161,.T.);
#7714=EDGE_CURVE('',#6221,#6222,#5162,.T.);
#7715=EDGE_CURVE('',#6222,#6223,#5163,.T.);
#7716=EDGE_CURVE('',#6223,#6224,#5164,.T.);
#7717=EDGE_CURVE('',#6224,#6225,#5165,.T.);
#7718=EDGE_CURVE('',#6225,#6226,#5166,.T.);
#7719=EDGE_CURVE('',#6226,#6227,#5167,.T.);
#7720=EDGE_CURVE('',#6227,#6228,#5168,.T.);
#7721=EDGE_CURVE('',#6228,#6229,#5169,.T.);
#7722=EDGE_CURVE('',#6229,#6230,#5170,.T.);
#7723=EDGE_CURVE('',#6230,#6231,#5171,.T.);
#7724=EDGE_CURVE('',#6231,#6232,#5172,.T.);
#7725=EDGE_CURVE('',#6232,#6233,#5173,.T.);
#7726=EDGE_CURVE('',#6233,#6234,#5174,.T.);
#7727=EDGE_CURVE('',#6234,#6235,#5175,.T.);
#7728=EDGE_CURVE('',#6235,#6236,#5176,.T.);
#7729=EDGE_CURVE('',#6236,#6237,#5177,.T.);
#7730=EDGE_CURVE('',#6237,#6238,#5178,.T.);
#7731=EDGE_CURVE('',#6238,#6239,#5179,.T.);
#7732=EDGE_CURVE('',#6239,#6240,#5180,.T.);
#7733=EDGE_CURVE('',#6240,#6241,#5181,.T.);
#7734=EDGE_CURVE('',#6241,#6242,#5182,.T.);
#7735=EDGE_CURVE('',#6242,#6243,#5183,.T.);
#7736=EDGE_CURVE('',#6243,#6244,#5184,.T.);
#7737=EDGE_CURVE('',#6244,#6245,#5185,.T.);
#7738=EDGE_CURVE('',#6245,#6246,#5186,.T.);
#7739=EDGE_CURVE('',#6246,#6247,#5187,.T.);
#7740=EDGE_CURVE('',#6247,#6248,#5188,.T.);
#7741=EDGE_CURVE('',#6248,#6249,#5189,.T.);
#7742=EDGE_CURVE('',#6249,#6250,#5190,.T.);
#7743=EDGE_CURVE('',#6250,#6251,#5191,.T.);
#7744=EDGE_CURVE('',#6251,#6252,#5192,.T.);
#7745=EDGE_CURVE('',#6252,#6253,#5193,.T.);
#7746=EDGE_CURVE('',#6253,#6254,#5194,.T.);
#7747=EDGE_CURVE('',#6254,#6255,#5195,.T.);
#7748=EDGE_CURVE('',#6255,#6256,#5196,.T.);
#7749=EDGE_CURVE('',#6256,#6257,#5197,.T.);
#7750=EDGE_CURVE('',#6257,#6258,#5198,.T.);
#7751=EDGE_CURVE('',#6258,#6259,#5199,.T.);
#7752=EDGE_CURVE('',#6259,#6260,#5200,.T.);
#7753=EDGE_CURVE('',#6260,#6261,#5201,.T.);
#7754=EDGE_CURVE('',#6261,#6182,#5202,.T.);
#7755=EDGE_CURVE('',#6262,#6262,#5203,.T.);
#7756=EDGE_CURVE('',#6262,#6181,#3578,.T.);
#7757=EDGE_CURVE('',#6183,#6100,#3579,.T.);
#7758=EDGE_CURVE('',#6101,#6182,#3580,.T.);
#7759=EDGE_CURVE('',#6261,#6102,#3581,.T.);
#7760=EDGE_CURVE('',#6103,#6260,#3582,.T.);
#7761=EDGE_CURVE('',#6259,#6104,#3583,.T.);
#7762=EDGE_CURVE('',#6105,#6258,#3584,.T.);
#7763=EDGE_CURVE('',#6257,#6106,#3585,.T.);
#7764=EDGE_CURVE('',#6107,#6256,#3586,.T.);
#7765=EDGE_CURVE('',#6255,#6108,#3587,.T.);
#7766=EDGE_CURVE('',#6109,#6254,#3588,.T.);
#7767=EDGE_CURVE('',#6253,#6110,#3589,.T.);
#7768=EDGE_CURVE('',#6111,#6252,#3590,.T.);
#7769=EDGE_CURVE('',#6251,#6112,#3591,.T.);
#7770=EDGE_CURVE('',#6113,#6250,#3592,.T.);
#7771=EDGE_CURVE('',#6249,#6114,#3593,.T.);
#7772=EDGE_CURVE('',#6115,#6248,#3594,.T.);
#7773=EDGE_CURVE('',#6247,#6116,#3595,.T.);
#7774=EDGE_CURVE('',#6117,#6246,#3596,.T.);
#7775=EDGE_CURVE('',#6245,#6118,#3597,.T.);
#7776=EDGE_CURVE('',#6119,#6244,#3598,.T.);
#7777=EDGE_CURVE('',#6243,#6120,#3599,.T.);
#7778=EDGE_CURVE('',#6121,#6242,#3600,.T.);
#7779=EDGE_CURVE('',#6241,#6122,#3601,.T.);
#7780=EDGE_CURVE('',#6123,#6240,#3602,.T.);
#7781=EDGE_CURVE('',#6239,#6124,#3603,.T.);
#7782=EDGE_CURVE('',#6125,#6238,#3604,.T.);
#7783=EDGE_CURVE('',#6237,#6126,#3605,.T.);
#7784=EDGE_CURVE('',#6127,#6236,#3606,.T.);
#7785=EDGE_CURVE('',#6235,#6128,#3607,.T.);
#7786=EDGE_CURVE('',#6129,#6234,#3608,.T.);
#7787=EDGE_CURVE('',#6233,#6130,#3609,.T.);
#7788=EDGE_CURVE('',#6131,#6232,#3610,.T.);
#7789=EDGE_CURVE('',#6231,#6132,#3611,.T.);
#7790=EDGE_CURVE('',#6133,#6230,#3612,.T.);
#7791=EDGE_CURVE('',#6229,#6134,#3613,.T.);
#7792=EDGE_CURVE('',#6135,#6228,#3614,.T.);
#7793=EDGE_CURVE('',#6227,#6136,#3615,.T.);
#7794=EDGE_CURVE('',#6137,#6226,#3616,.T.);
#7795=EDGE_CURVE('',#6225,#6138,#3617,.T.);
#7796=EDGE_CURVE('',#6139,#6224,#3618,.T.);
#7797=EDGE_CURVE('',#6223,#6140,#3619,.T.);
#7798=EDGE_CURVE('',#6141,#6222,#3620,.T.);
#7799=EDGE_CURVE('',#6221,#6142,#3621,.T.);
#7800=EDGE_CURVE('',#6143,#6220,#3622,.T.);
#7801=EDGE_CURVE('',#6219,#6144,#3623,.T.);
#7802=EDGE_CURVE('',#6145,#6218,#3624,.T.);
#7803=EDGE_CURVE('',#6217,#6146,#3625,.T.);
#7804=EDGE_CURVE('',#6147,#6216,#3626,.T.);
#7805=EDGE_CURVE('',#6215,#6148,#3627,.T.);
#7806=EDGE_CURVE('',#6149,#6214,#3628,.T.);
#7807=EDGE_CURVE('',#6213,#6150,#3629,.T.);
#7808=EDGE_CURVE('',#6151,#6212,#3630,.T.);
#7809=EDGE_CURVE('',#6211,#6152,#3631,.T.);
#7810=EDGE_CURVE('',#6153,#6210,#3632,.T.);
#7811=EDGE_CURVE('',#6209,#6154,#3633,.T.);
#7812=EDGE_CURVE('',#6155,#6208,#3634,.T.);
#7813=EDGE_CURVE('',#6207,#6156,#3635,.T.);
#7814=EDGE_CURVE('',#6157,#6206,#3636,.T.);
#7815=EDGE_CURVE('',#6205,#6158,#3637,.T.);
#7816=EDGE_CURVE('',#6159,#6204,#3638,.T.);
#7817=EDGE_CURVE('',#6203,#6160,#3639,.T.);
#7818=EDGE_CURVE('',#6161,#6202,#3640,.T.);
#7819=EDGE_CURVE('',#6201,#6162,#3641,.T.);
#7820=EDGE_CURVE('',#6163,#6200,#3642,.T.);
#7821=EDGE_CURVE('',#6199,#6164,#3643,.T.);
#7822=EDGE_CURVE('',#6165,#6198,#3644,.T.);
#7823=EDGE_CURVE('',#6197,#6166,#3645,.T.);
#7824=EDGE_CURVE('',#6167,#6196,#3646,.T.);
#7825=EDGE_CURVE('',#6195,#6168,#3647,.T.);
#7826=EDGE_CURVE('',#6169,#6194,#3648,.T.);
#7827=EDGE_CURVE('',#6193,#6170,#3649,.T.);
#7828=EDGE_CURVE('',#6171,#6192,#3650,.T.);
#7829=EDGE_CURVE('',#6191,#6172,#3651,.T.);
#7830=EDGE_CURVE('',#6173,#6190,#3652,.T.);
#7831=EDGE_CURVE('',#6189,#6174,#3653,.T.);
#7832=EDGE_CURVE('',#6175,#6188,#3654,.T.);
#7833=EDGE_CURVE('',#6187,#6176,#3655,.T.);
#7834=EDGE_CURVE('',#6177,#6186,#3656,.T.);
#7835=EDGE_CURVE('',#6179,#6184,#3657,.T.);
#7836=EDGE_CURVE('',#6185,#6178,#3658,.T.);
#7837=EDGE_CURVE('',#6263,#6263,#5204,.T.);
#7838=EDGE_CURVE('',#6264,#6264,#5205,.T.);
#7839=EDGE_CURVE('',#6264,#6263,#3659,.T.);
#7840=EDGE_CURVE('',#6265,#6265,#5206,.T.);
#7841=EDGE_CURVE('',#6265,#6264,#3660,.T.);
#7842=EDGE_CURVE('',#6266,#6266,#5207,.T.);
#7843=EDGE_CURVE('',#6266,#6265,#3661,.T.);
#7844=EDGE_CURVE('',#6267,#6267,#5208,.T.);
#7845=EDGE_CURVE('',#6268,#6268,#5209,.F.);
#7846=EDGE_CURVE('',#6268,#6267,#3662,.T.);
#7847=EDGE_CURVE('',#6269,#6269,#5210,.F.);
#7848=EDGE_CURVE('',#6269,#6268,#3663,.T.);
#7849=EDGE_CURVE('',#6270,#6270,#5211,.T.);
#7850=EDGE_CURVE('',#6270,#6269,#3664,.T.);
#7851=EDGE_CURVE('',#6271,#6272,#3665,.T.);
#7852=EDGE_CURVE('',#6272,#6273,#3666,.T.);
#7853=EDGE_CURVE('',#6273,#6274,#3667,.T.);
#7854=EDGE_CURVE('',#6271,#6274,#3668,.T.);
#7855=EDGE_CURVE('',#6272,#6275,#3669,.T.);
#7856=EDGE_CURVE('',#6275,#6276,#3670,.T.);
#7857=EDGE_CURVE('',#6276,#6273,#3671,.T.);
#7858=EDGE_CURVE('',#6275,#6277,#3672,.T.);
#7859=EDGE_CURVE('',#6277,#6278,#3673,.T.);
#7860=EDGE_CURVE('',#6278,#6276,#3674,.T.);
#7861=EDGE_CURVE('',#6277,#6279,#3675,.T.);
#7862=EDGE_CURVE('',#6279,#6280,#3676,.T.);
#7863=EDGE_CURVE('',#6280,#6278,#3677,.T.);
#7864=EDGE_CURVE('',#6279,#6281,#3678,.T.);
#7865=EDGE_CURVE('',#6281,#6282,#3679,.T.);
#7866=EDGE_CURVE('',#6282,#6280,#3680,.T.);
#7867=EDGE_CURVE('',#6281,#6271,#3681,.T.);
#7868=EDGE_CURVE('',#6274,#6282,#3682,.T.);
#7869=EDGE_CURVE('',#6283,#6283,#5212,.T.);
#7870=EDGE_CURVE('',#6283,#6284,#3683,.T.);
#7871=EDGE_CURVE('',#6284,#6284,#5213,.T.);
#7872=EDGE_CURVE('',#6285,#6285,#5214,.T.);
#7873=EDGE_CURVE('',#6286,#6286,#5215,.T.);
#7874=EDGE_CURVE('',#6287,#6287,#5216,.T.);
#7875=EDGE_CURVE('',#6288,#6288,#5217,.T.);
#7876=EDGE_CURVE('',#6285,#6287,#3684,.T.);
#7877=EDGE_CURVE('',#6288,#6289,#3685,.T.);
#7878=EDGE_CURVE('',#6289,#6289,#5218,.T.);
#7879=EDGE_CURVE('',#6290,#6290,#5219,.T.);
#7880=EDGE_CURVE('',#6291,#6291,#5220,.T.);
#7881=EDGE_CURVE('',#6292,#6292,#5221,.T.);
#7882=EDGE_CURVE('',#6293,#6293,#5222,.T.);
#7883=EDGE_CURVE('',#6290,#6292,#3686,.T.);
#7884=EDGE_CURVE('',#6293,#6294,#3687,.T.);
#7885=EDGE_CURVE('',#6294,#6294,#5223,.T.);
#7886=EDGE_CURVE('',#6295,#6295,#5224,.T.);
#7887=EDGE_CURVE('',#6296,#6296,#5225,.T.);
#7888=EDGE_CURVE('',#6296,#6286,#3688,.T.);
#7889=EDGE_CURVE('',#6297,#6297,#5226,.T.);
#7890=EDGE_CURVE('',#6298,#6298,#5227,.T.);
#7891=EDGE_CURVE('',#6297,#6291,#3689,.T.);
#7892=EDGE_CURVE('',#6295,#6298,#3690,.T.);
#7893=EDGE_CURVE('',#6299,#6300,#3691,.T.);
#7894=EDGE_CURVE('',#6299,#6300,#5228,.T.);
#7895=EDGE_CURVE('',#6301,#6302,#575,.T.);
#7896=EDGE_CURVE('',#6303,#6301,#5229,.T.);
#7897=EDGE_CURVE('',#6304,#6303,#576,.T.);
#7898=EDGE_CURVE('',#6300,#6304,#577,.T.);
#7899=EDGE_CURVE('',#6302,#6299,#578,.T.);
#7900=EDGE_CURVE('',#6302,#6305,#3692,.T.);
#7901=EDGE_CURVE('',#6306,#6305,#579,.T.);
#7902=EDGE_CURVE('',#6307,#6306,#580,.T.);
#7903=EDGE_CURVE('',#6305,#6307,#581,.T.);
#7904=EDGE_CURVE('',#6303,#6301,#3693,.T.);
#7905=EDGE_CURVE('',#6308,#6308,#5230,.T.);
#7906=EDGE_CURVE('',#6308,#6304,#3694,.T.);
#7907=EDGE_CURVE('',#6302,#6309,#3695,.T.);
#7908=EDGE_CURVE('',#6309,#6309,#5231,.T.);
#7909=EDGE_CURVE('',#6310,#6310,#5232,.T.);
#7910=EDGE_CURVE('',#6310,#6307,#3696,.T.);
#7911=EDGE_CURVE('',#6305,#6311,#3697,.T.);
#7912=EDGE_CURVE('',#6311,#6311,#5233,.T.);
#7913=EDGE_CURVE('',#6312,#6313,#3698,.T.);
#7914=EDGE_CURVE('',#6312,#6314,#3699,.T.);
#7915=EDGE_CURVE('',#6314,#6315,#3700,.T.);
#7916=EDGE_CURVE('',#6313,#6315,#3701,.T.);
#7917=EDGE_CURVE('',#6316,#6312,#3702,.T.);
#7918=EDGE_CURVE('',#6316,#6317,#3703,.T.);
#7919=EDGE_CURVE('',#6317,#6314,#3704,.T.);
#7920=EDGE_CURVE('',#6318,#6316,#3705,.T.);
#7921=EDGE_CURVE('',#6318,#6319,#3706,.T.);
#7922=EDGE_CURVE('',#6319,#6317,#3707,.T.);
#7923=EDGE_CURVE('',#6320,#6318,#3708,.T.);
#7924=EDGE_CURVE('',#6320,#6321,#3709,.T.);
#7925=EDGE_CURVE('',#6321,#6319,#3710,.T.);
#7926=EDGE_CURVE('',#6322,#6320,#3711,.T.);
#7927=EDGE_CURVE('',#6322,#6323,#3712,.T.);
#7928=EDGE_CURVE('',#6323,#6321,#3713,.T.);
#7929=EDGE_CURVE('',#6313,#6322,#3714,.T.);
#7930=EDGE_CURVE('',#6315,#6323,#3715,.T.);
#7931=EDGE_CURVE('',#6324,#6324,#5234,.T.);
#7932=EDGE_CURVE('',#6325,#6325,#5235,.T.);
#7933=EDGE_CURVE('',#6325,#6324,#3716,.T.);
#7934=EDGE_CURVE('',#6326,#6326,#5236,.F.);
#7935=EDGE_CURVE('',#6326,#6325,#3717,.T.);
#7936=EDGE_CURVE('',#6327,#6327,#5237,.T.);
#7937=EDGE_CURVE('',#6327,#6326,#3718,.T.);
#7938=ORIENTED_EDGE('',*,*,#6328,.F.);
#7939=ORIENTED_EDGE('',*,*,#6329,.T.);
#7940=ORIENTED_EDGE('',*,*,#6330,.F.);
#7941=ORIENTED_EDGE('',*,*,#6329,.F.);
#7942=ORIENTED_EDGE('',*,*,#6328,.T.);
#7943=ORIENTED_EDGE('',*,*,#6331,.F.);
#7944=ORIENTED_EDGE('',*,*,#6332,.T.);
#7945=ORIENTED_EDGE('',*,*,#6333,.F.);
#7946=ORIENTED_EDGE('',*,*,#6332,.F.);
#7947=ORIENTED_EDGE('',*,*,#6331,.T.);
#7948=ORIENTED_EDGE('',*,*,#6334,.F.);
#7949=ORIENTED_EDGE('',*,*,#6335,.T.);
#7950=ORIENTED_EDGE('',*,*,#6336,.F.);
#7951=ORIENTED_EDGE('',*,*,#6335,.F.);
#7952=ORIENTED_EDGE('',*,*,#6334,.T.);
#7953=ORIENTED_EDGE('',*,*,#6337,.F.);
#7954=ORIENTED_EDGE('',*,*,#6338,.T.);
#7955=ORIENTED_EDGE('',*,*,#6339,.F.);
#7956=ORIENTED_EDGE('',*,*,#6338,.F.);
#7957=ORIENTED_EDGE('',*,*,#6337,.T.);
#7958=ORIENTED_EDGE('',*,*,#6340,.F.);
#7959=ORIENTED_EDGE('',*,*,#6341,.T.);
#7960=ORIENTED_EDGE('',*,*,#6342,.F.);
#7961=ORIENTED_EDGE('',*,*,#6341,.F.);
#7962=ORIENTED_EDGE('',*,*,#6340,.T.);
#7963=ORIENTED_EDGE('',*,*,#6343,.F.);
#7964=ORIENTED_EDGE('',*,*,#6344,.T.);
#7965=ORIENTED_EDGE('',*,*,#6345,.F.);
#7966=ORIENTED_EDGE('',*,*,#6344,.F.);
#7967=ORIENTED_EDGE('',*,*,#6343,.T.);
#7968=ORIENTED_EDGE('',*,*,#6346,.F.);
#7969=ORIENTED_EDGE('',*,*,#6347,.T.);
#7970=ORIENTED_EDGE('',*,*,#6348,.F.);
#7971=ORIENTED_EDGE('',*,*,#6347,.F.);
#7972=ORIENTED_EDGE('',*,*,#6346,.T.);
#7973=ORIENTED_EDGE('',*,*,#6349,.F.);
#7974=ORIENTED_EDGE('',*,*,#6350,.T.);
#7975=ORIENTED_EDGE('',*,*,#6351,.F.);
#7976=ORIENTED_EDGE('',*,*,#6350,.F.);
#7977=ORIENTED_EDGE('',*,*,#6349,.T.);
#7978=ORIENTED_EDGE('',*,*,#6352,.F.);
#7979=ORIENTED_EDGE('',*,*,#6353,.T.);
#7980=ORIENTED_EDGE('',*,*,#6354,.F.);
#7981=ORIENTED_EDGE('',*,*,#6353,.F.);
#7982=ORIENTED_EDGE('',*,*,#6352,.T.);
#7983=ORIENTED_EDGE('',*,*,#6355,.F.);
#7984=ORIENTED_EDGE('',*,*,#6356,.T.);
#7985=ORIENTED_EDGE('',*,*,#6357,.F.);
#7986=ORIENTED_EDGE('',*,*,#6356,.F.);
#7987=ORIENTED_EDGE('',*,*,#6355,.T.);
#7988=ORIENTED_EDGE('',*,*,#6358,.F.);
#7989=ORIENTED_EDGE('',*,*,#6359,.T.);
#7990=ORIENTED_EDGE('',*,*,#6360,.F.);
#7991=ORIENTED_EDGE('',*,*,#6359,.F.);
#7992=ORIENTED_EDGE('',*,*,#6358,.T.);
#7993=ORIENTED_EDGE('',*,*,#6361,.F.);
#7994=ORIENTED_EDGE('',*,*,#6362,.T.);
#7995=ORIENTED_EDGE('',*,*,#6363,.F.);
#7996=ORIENTED_EDGE('',*,*,#6362,.F.);
#7997=ORIENTED_EDGE('',*,*,#6361,.T.);
#7998=ORIENTED_EDGE('',*,*,#6364,.F.);
#7999=ORIENTED_EDGE('',*,*,#6365,.T.);
#8000=ORIENTED_EDGE('',*,*,#6366,.F.);
#8001=ORIENTED_EDGE('',*,*,#6365,.F.);
#8002=ORIENTED_EDGE('',*,*,#6364,.T.);
#8003=ORIENTED_EDGE('',*,*,#6367,.F.);
#8004=ORIENTED_EDGE('',*,*,#6368,.T.);
#8005=ORIENTED_EDGE('',*,*,#6369,.F.);
#8006=ORIENTED_EDGE('',*,*,#6368,.F.);
#8007=ORIENTED_EDGE('',*,*,#6367,.T.);
#8008=ORIENTED_EDGE('',*,*,#6370,.T.);
#8009=ORIENTED_EDGE('',*,*,#6371,.T.);
#8010=ORIENTED_EDGE('',*,*,#6372,.F.);
#8011=ORIENTED_EDGE('',*,*,#6373,.F.);
#8012=ORIENTED_EDGE('',*,*,#6374,.T.);
#8013=ORIENTED_EDGE('',*,*,#6373,.T.);
#8014=ORIENTED_EDGE('',*,*,#6375,.F.);
#8015=ORIENTED_EDGE('',*,*,#6376,.F.);
#8016=ORIENTED_EDGE('',*,*,#6377,.T.);
#8017=ORIENTED_EDGE('',*,*,#6376,.T.);
#8018=ORIENTED_EDGE('',*,*,#6378,.F.);
#8019=ORIENTED_EDGE('',*,*,#6379,.F.);
#8020=ORIENTED_EDGE('',*,*,#6380,.T.);
#8021=ORIENTED_EDGE('',*,*,#6379,.T.);
#8022=ORIENTED_EDGE('',*,*,#6381,.F.);
#8023=ORIENTED_EDGE('',*,*,#6371,.F.);
#8024=ORIENTED_EDGE('',*,*,#6381,.T.);
#8025=ORIENTED_EDGE('',*,*,#6378,.T.);
#8026=ORIENTED_EDGE('',*,*,#6375,.T.);
#8027=ORIENTED_EDGE('',*,*,#6372,.T.);
#8028=ORIENTED_EDGE('',*,*,#6336,.T.);
#8029=ORIENTED_EDGE('',*,*,#6339,.T.);
#8030=ORIENTED_EDGE('',*,*,#6348,.T.);
#8031=ORIENTED_EDGE('',*,*,#6351,.T.);
#8032=ORIENTED_EDGE('',*,*,#6354,.T.);
#8033=ORIENTED_EDGE('',*,*,#6357,.T.);
#8034=ORIENTED_EDGE('',*,*,#6360,.T.);
#8035=ORIENTED_EDGE('',*,*,#6363,.T.);
#8036=ORIENTED_EDGE('',*,*,#6366,.T.);
#8037=ORIENTED_EDGE('',*,*,#6369,.T.);
#8038=ORIENTED_EDGE('',*,*,#6345,.T.);
#8039=ORIENTED_EDGE('',*,*,#6342,.T.);
#8040=ORIENTED_EDGE('',*,*,#6333,.T.);
#8041=ORIENTED_EDGE('',*,*,#6330,.T.);
#8042=ORIENTED_EDGE('',*,*,#6380,.F.);
#8043=ORIENTED_EDGE('',*,*,#6370,.F.);
#8044=ORIENTED_EDGE('',*,*,#6374,.F.);
#8045=ORIENTED_EDGE('',*,*,#6377,.F.);
#8046=ORIENTED_EDGE('',*,*,#6382,.T.);
#8047=ORIENTED_EDGE('',*,*,#6383,.T.);
#8048=ORIENTED_EDGE('',*,*,#6384,.F.);
#8049=ORIENTED_EDGE('',*,*,#6385,.F.);
#8050=ORIENTED_EDGE('',*,*,#6386,.T.);
#8051=ORIENTED_EDGE('',*,*,#6385,.T.);
#8052=ORIENTED_EDGE('',*,*,#6387,.F.);
#8053=ORIENTED_EDGE('',*,*,#6388,.F.);
#8054=ORIENTED_EDGE('',*,*,#6389,.T.);
#8055=ORIENTED_EDGE('',*,*,#6388,.T.);
#8056=ORIENTED_EDGE('',*,*,#6390,.F.);
#8057=ORIENTED_EDGE('',*,*,#6391,.F.);
#8058=ORIENTED_EDGE('',*,*,#6392,.T.);
#8059=ORIENTED_EDGE('',*,*,#6391,.T.);
#8060=ORIENTED_EDGE('',*,*,#6393,.F.);
#8061=ORIENTED_EDGE('',*,*,#6383,.F.);
#8062=ORIENTED_EDGE('',*,*,#6393,.T.);
#8063=ORIENTED_EDGE('',*,*,#6390,.T.);
#8064=ORIENTED_EDGE('',*,*,#6387,.T.);
#8065=ORIENTED_EDGE('',*,*,#6384,.T.);
#8066=ORIENTED_EDGE('',*,*,#6392,.F.);
#8067=ORIENTED_EDGE('',*,*,#6382,.F.);
#8068=ORIENTED_EDGE('',*,*,#6386,.F.);
#8069=ORIENTED_EDGE('',*,*,#6389,.F.);
#8070=ORIENTED_EDGE('',*,*,#6394,.T.);
#8071=ORIENTED_EDGE('',*,*,#6395,.T.);
#8072=ORIENTED_EDGE('',*,*,#6396,.F.);
#8073=ORIENTED_EDGE('',*,*,#6397,.F.);
#8074=ORIENTED_EDGE('',*,*,#6398,.T.);
#8075=ORIENTED_EDGE('',*,*,#6397,.T.);
#8076=ORIENTED_EDGE('',*,*,#6399,.F.);
#8077=ORIENTED_EDGE('',*,*,#6400,.F.);
#8078=ORIENTED_EDGE('',*,*,#6401,.T.);
#8079=ORIENTED_EDGE('',*,*,#6400,.T.);
#8080=ORIENTED_EDGE('',*,*,#6402,.F.);
#8081=ORIENTED_EDGE('',*,*,#6403,.F.);
#8082=ORIENTED_EDGE('',*,*,#6404,.T.);
#8083=ORIENTED_EDGE('',*,*,#6403,.T.);
#8084=ORIENTED_EDGE('',*,*,#6405,.F.);
#8085=ORIENTED_EDGE('',*,*,#6395,.F.);
#8086=ORIENTED_EDGE('',*,*,#6405,.T.);
#8087=ORIENTED_EDGE('',*,*,#6402,.T.);
#8088=ORIENTED_EDGE('',*,*,#6399,.T.);
#8089=ORIENTED_EDGE('',*,*,#6396,.T.);
#8090=ORIENTED_EDGE('',*,*,#6404,.F.);
#8091=ORIENTED_EDGE('',*,*,#6394,.F.);
#8092=ORIENTED_EDGE('',*,*,#6398,.F.);
#8093=ORIENTED_EDGE('',*,*,#6401,.F.);
#8094=ORIENTED_EDGE('',*,*,#6406,.F.);
#8095=ORIENTED_EDGE('',*,*,#6407,.T.);
#8096=ORIENTED_EDGE('',*,*,#6408,.F.);
#8097=ORIENTED_EDGE('',*,*,#6407,.F.);
#8098=ORIENTED_EDGE('',*,*,#6409,.F.);
#8099=ORIENTED_EDGE('',*,*,#6410,.T.);
#8100=ORIENTED_EDGE('',*,*,#6411,.F.);
#8101=ORIENTED_EDGE('',*,*,#6410,.F.);
#8102=ORIENTED_EDGE('',*,*,#6412,.F.);
#8103=ORIENTED_EDGE('',*,*,#6413,.T.);
#8104=ORIENTED_EDGE('',*,*,#6414,.F.);
#8105=ORIENTED_EDGE('',*,*,#6413,.F.);
#8106=ORIENTED_EDGE('',*,*,#6415,.F.);
#8107=ORIENTED_EDGE('',*,*,#6416,.T.);
#8108=ORIENTED_EDGE('',*,*,#6417,.F.);
#8109=ORIENTED_EDGE('',*,*,#6416,.F.);
#8110=ORIENTED_EDGE('',*,*,#6418,.F.);
#8111=ORIENTED_EDGE('',*,*,#6419,.T.);
#8112=ORIENTED_EDGE('',*,*,#6420,.F.);
#8113=ORIENTED_EDGE('',*,*,#6419,.F.);
#8114=ORIENTED_EDGE('',*,*,#6421,.F.);
#8115=ORIENTED_EDGE('',*,*,#6422,.T.);
#8116=ORIENTED_EDGE('',*,*,#6423,.F.);
#8117=ORIENTED_EDGE('',*,*,#6422,.F.);
#8118=ORIENTED_EDGE('',*,*,#6424,.F.);
#8119=ORIENTED_EDGE('',*,*,#6425,.T.);
#8120=ORIENTED_EDGE('',*,*,#6426,.F.);
#8121=ORIENTED_EDGE('',*,*,#6425,.F.);
#8122=ORIENTED_EDGE('',*,*,#6427,.F.);
#8123=ORIENTED_EDGE('',*,*,#6428,.T.);
#8124=ORIENTED_EDGE('',*,*,#6429,.F.);
#8125=ORIENTED_EDGE('',*,*,#6428,.F.);
#8126=ORIENTED_EDGE('',*,*,#6430,.F.);
#8127=ORIENTED_EDGE('',*,*,#6431,.T.);
#8128=ORIENTED_EDGE('',*,*,#6432,.F.);
#8129=ORIENTED_EDGE('',*,*,#6431,.F.);
#8130=ORIENTED_EDGE('',*,*,#6433,.F.);
#8131=ORIENTED_EDGE('',*,*,#6434,.F.);
#8132=ORIENTED_EDGE('',*,*,#6435,.T.);
#8133=ORIENTED_EDGE('',*,*,#6436,.F.);
#8134=ORIENTED_EDGE('',*,*,#6423,.T.);
#8135=ORIENTED_EDGE('',*,*,#6432,.T.);
#8136=ORIENTED_EDGE('',*,*,#6437,.F.);
#8137=ORIENTED_EDGE('',*,*,#6438,.F.);
#8138=ORIENTED_EDGE('',*,*,#6439,.F.);
#8139=ORIENTED_EDGE('',*,*,#6440,.F.);
#8140=ORIENTED_EDGE('',*,*,#6426,.T.);
#8141=ORIENTED_EDGE('',*,*,#6429,.T.);
#8142=ORIENTED_EDGE('',*,*,#6441,.F.);
#8143=ORIENTED_EDGE('',*,*,#6439,.T.);
#8144=ORIENTED_EDGE('',*,*,#6442,.F.);
#8145=ORIENTED_EDGE('',*,*,#6443,.F.);
#8146=ORIENTED_EDGE('',*,*,#6444,.F.);
#8147=ORIENTED_EDGE('',*,*,#6445,.T.);
#8148=ORIENTED_EDGE('',*,*,#6446,.F.);
#8149=ORIENTED_EDGE('',*,*,#6435,.F.);
#8150=ORIENTED_EDGE('',*,*,#6447,.T.);
#8151=ORIENTED_EDGE('',*,*,#6448,.F.);
#8152=ORIENTED_EDGE('',*,*,#6449,.F.);
#8153=ORIENTED_EDGE('',*,*,#6440,.T.);
#8154=ORIENTED_EDGE('',*,*,#6441,.T.);
#8155=ORIENTED_EDGE('',*,*,#6450,.T.);
#8156=ORIENTED_EDGE('',*,*,#6444,.T.);
#8157=ORIENTED_EDGE('',*,*,#6434,.T.);
#8158=ORIENTED_EDGE('',*,*,#6418,.T.);
#8159=ORIENTED_EDGE('',*,*,#6415,.T.);
#8160=ORIENTED_EDGE('',*,*,#6412,.T.);
#8161=ORIENTED_EDGE('',*,*,#6409,.T.);
#8162=ORIENTED_EDGE('',*,*,#6406,.T.);
#8163=ORIENTED_EDGE('',*,*,#6433,.T.);
#8164=ORIENTED_EDGE('',*,*,#6451,.T.);
#8165=ORIENTED_EDGE('',*,*,#6452,.F.);
#8166=ORIENTED_EDGE('',*,*,#6447,.F.);
#8167=ORIENTED_EDGE('',*,*,#6453,.T.);
#8168=ORIENTED_EDGE('',*,*,#6454,.F.);
#8169=ORIENTED_EDGE('',*,*,#6451,.F.);
#8170=ORIENTED_EDGE('',*,*,#6436,.T.);
#8171=ORIENTED_EDGE('',*,*,#6446,.T.);
#8172=ORIENTED_EDGE('',*,*,#6455,.T.);
#8173=ORIENTED_EDGE('',*,*,#6442,.T.);
#8174=ORIENTED_EDGE('',*,*,#6438,.T.);
#8175=ORIENTED_EDGE('',*,*,#6420,.T.);
#8176=ORIENTED_EDGE('',*,*,#6417,.T.);
#8177=ORIENTED_EDGE('',*,*,#6414,.T.);
#8178=ORIENTED_EDGE('',*,*,#6411,.T.);
#8179=ORIENTED_EDGE('',*,*,#6408,.T.);
#8180=ORIENTED_EDGE('',*,*,#6437,.T.);
#8181=ORIENTED_EDGE('',*,*,#6449,.T.);
#8182=ORIENTED_EDGE('',*,*,#6456,.F.);
#8183=ORIENTED_EDGE('',*,*,#6453,.F.);
#8184=ORIENTED_EDGE('',*,*,#6456,.T.);
#8185=ORIENTED_EDGE('',*,*,#6448,.T.);
#8186=ORIENTED_EDGE('',*,*,#6452,.T.);
#8187=ORIENTED_EDGE('',*,*,#6454,.T.);
#8188=ORIENTED_EDGE('',*,*,#6455,.F.);
#8189=ORIENTED_EDGE('',*,*,#6445,.F.);
#8190=ORIENTED_EDGE('',*,*,#6450,.F.);
#8191=ORIENTED_EDGE('',*,*,#6443,.T.);
#8192=ORIENTED_EDGE('',*,*,#6421,.T.);
#8193=ORIENTED_EDGE('',*,*,#6424,.T.);
#8194=ORIENTED_EDGE('',*,*,#6427,.T.);
#8195=ORIENTED_EDGE('',*,*,#6430,.T.);
#8196=ORIENTED_EDGE('',*,*,#6457,.F.);
#8197=ORIENTED_EDGE('',*,*,#6458,.T.);
#8198=ORIENTED_EDGE('',*,*,#6459,.T.);
#8199=ORIENTED_EDGE('',*,*,#6458,.F.);
#8200=ORIENTED_EDGE('',*,*,#6460,.F.);
#8201=ORIENTED_EDGE('',*,*,#6461,.T.);
#8202=ORIENTED_EDGE('',*,*,#6462,.T.);
#8203=ORIENTED_EDGE('',*,*,#6461,.F.);
#8204=ORIENTED_EDGE('',*,*,#6460,.T.);
#8205=ORIENTED_EDGE('',*,*,#6457,.T.);
#8206=ORIENTED_EDGE('',*,*,#6462,.F.);
#8207=ORIENTED_EDGE('',*,*,#6459,.F.);
#8208=ORIENTED_EDGE('',*,*,#6463,.F.);
#8209=ORIENTED_EDGE('',*,*,#6464,.F.);
#8210=ORIENTED_EDGE('',*,*,#6465,.F.);
#8211=ORIENTED_EDGE('',*,*,#6466,.F.);
#8212=ORIENTED_EDGE('',*,*,#6467,.F.);
#8213=ORIENTED_EDGE('',*,*,#6468,.F.);
#8214=ORIENTED_EDGE('',*,*,#6469,.F.);
#8215=ORIENTED_EDGE('',*,*,#6470,.F.);
#8216=ORIENTED_EDGE('',*,*,#6471,.F.);
#8217=ORIENTED_EDGE('',*,*,#6472,.F.);
#8218=ORIENTED_EDGE('',*,*,#6473,.F.);
#8219=ORIENTED_EDGE('',*,*,#6474,.F.);
#8220=ORIENTED_EDGE('',*,*,#6475,.F.);
#8221=ORIENTED_EDGE('',*,*,#6476,.F.);
#8222=ORIENTED_EDGE('',*,*,#6477,.F.);
#8223=ORIENTED_EDGE('',*,*,#6478,.F.);
#8224=ORIENTED_EDGE('',*,*,#6464,.T.);
#8225=ORIENTED_EDGE('',*,*,#6479,.F.);
#8226=ORIENTED_EDGE('',*,*,#6476,.T.);
#8227=ORIENTED_EDGE('',*,*,#6480,.F.);
#8228=ORIENTED_EDGE('',*,*,#6472,.T.);
#8229=ORIENTED_EDGE('',*,*,#6481,.F.);
#8230=ORIENTED_EDGE('',*,*,#6468,.T.);
#8231=ORIENTED_EDGE('',*,*,#6482,.F.);
#8232=ORIENTED_EDGE('',*,*,#6483,.F.);
#8233=ORIENTED_EDGE('',*,*,#6473,.T.);
#8234=ORIENTED_EDGE('',*,*,#6480,.T.);
#8235=ORIENTED_EDGE('',*,*,#6475,.T.);
#8236=ORIENTED_EDGE('',*,*,#6484,.F.);
#8237=ORIENTED_EDGE('',*,*,#6469,.T.);
#8238=ORIENTED_EDGE('',*,*,#6481,.T.);
#8239=ORIENTED_EDGE('',*,*,#6471,.T.);
#8240=ORIENTED_EDGE('',*,*,#6485,.F.);
#8241=ORIENTED_EDGE('',*,*,#6463,.T.);
#8242=ORIENTED_EDGE('',*,*,#6486,.F.);
#8243=ORIENTED_EDGE('',*,*,#6477,.T.);
#8244=ORIENTED_EDGE('',*,*,#6479,.T.);
#8245=ORIENTED_EDGE('',*,*,#6465,.T.);
#8246=ORIENTED_EDGE('',*,*,#6482,.T.);
#8247=ORIENTED_EDGE('',*,*,#6467,.T.);
#8248=ORIENTED_EDGE('',*,*,#6487,.F.);
#8249=ORIENTED_EDGE('',*,*,#6488,.F.);
#8250=ORIENTED_EDGE('',*,*,#6489,.T.);
#8251=ORIENTED_EDGE('',*,*,#6490,.F.);
#8252=ORIENTED_EDGE('',*,*,#6489,.F.);
#8253=ORIENTED_EDGE('',*,*,#6488,.T.);
#8254=ORIENTED_EDGE('',*,*,#6491,.T.);
#8255=ORIENTED_EDGE('',*,*,#6491,.F.);
#8256=ORIENTED_EDGE('',*,*,#6492,.T.);
#8257=ORIENTED_EDGE('',*,*,#6483,.T.);
#8258=ORIENTED_EDGE('',*,*,#6492,.F.);
#8259=ORIENTED_EDGE('',*,*,#6466,.T.);
#8260=ORIENTED_EDGE('',*,*,#6487,.T.);
#8261=ORIENTED_EDGE('',*,*,#6470,.T.);
#8262=ORIENTED_EDGE('',*,*,#6485,.T.);
#8263=ORIENTED_EDGE('',*,*,#6474,.T.);
#8264=ORIENTED_EDGE('',*,*,#6484,.T.);
#8265=ORIENTED_EDGE('',*,*,#6478,.T.);
#8266=ORIENTED_EDGE('',*,*,#6486,.T.);
#8267=ORIENTED_EDGE('',*,*,#6490,.T.);
#8268=ORIENTED_EDGE('',*,*,#6493,.F.);
#8269=ORIENTED_EDGE('',*,*,#6494,.F.);
#8270=ORIENTED_EDGE('',*,*,#6495,.F.);
#8271=ORIENTED_EDGE('',*,*,#6496,.F.);
#8272=ORIENTED_EDGE('',*,*,#6497,.F.);
#8273=ORIENTED_EDGE('',*,*,#6498,.F.);
#8274=ORIENTED_EDGE('',*,*,#6499,.F.);
#8275=ORIENTED_EDGE('',*,*,#6500,.F.);
#8276=ORIENTED_EDGE('',*,*,#6501,.F.);
#8277=ORIENTED_EDGE('',*,*,#6502,.F.);
#8278=ORIENTED_EDGE('',*,*,#6503,.F.);
#8279=ORIENTED_EDGE('',*,*,#6504,.F.);
#8280=ORIENTED_EDGE('',*,*,#6505,.F.);
#8281=ORIENTED_EDGE('',*,*,#6506,.F.);
#8282=ORIENTED_EDGE('',*,*,#6507,.F.);
#8283=ORIENTED_EDGE('',*,*,#6508,.F.);
#8284=ORIENTED_EDGE('',*,*,#6494,.T.);
#8285=ORIENTED_EDGE('',*,*,#6509,.F.);
#8286=ORIENTED_EDGE('',*,*,#6506,.T.);
#8287=ORIENTED_EDGE('',*,*,#6510,.F.);
#8288=ORIENTED_EDGE('',*,*,#6502,.T.);
#8289=ORIENTED_EDGE('',*,*,#6511,.F.);
#8290=ORIENTED_EDGE('',*,*,#6498,.T.);
#8291=ORIENTED_EDGE('',*,*,#6512,.F.);
#8292=ORIENTED_EDGE('',*,*,#6513,.T.);
#8293=ORIENTED_EDGE('',*,*,#6503,.T.);
#8294=ORIENTED_EDGE('',*,*,#6510,.T.);
#8295=ORIENTED_EDGE('',*,*,#6505,.T.);
#8296=ORIENTED_EDGE('',*,*,#6514,.F.);
#8297=ORIENTED_EDGE('',*,*,#6499,.T.);
#8298=ORIENTED_EDGE('',*,*,#6511,.T.);
#8299=ORIENTED_EDGE('',*,*,#6501,.T.);
#8300=ORIENTED_EDGE('',*,*,#6515,.F.);
#8301=ORIENTED_EDGE('',*,*,#6493,.T.);
#8302=ORIENTED_EDGE('',*,*,#6516,.F.);
#8303=ORIENTED_EDGE('',*,*,#6507,.T.);
#8304=ORIENTED_EDGE('',*,*,#6509,.T.);
#8305=ORIENTED_EDGE('',*,*,#6495,.T.);
#8306=ORIENTED_EDGE('',*,*,#6512,.T.);
#8307=ORIENTED_EDGE('',*,*,#6497,.T.);
#8308=ORIENTED_EDGE('',*,*,#6517,.F.);
#8309=ORIENTED_EDGE('',*,*,#6513,.F.);
#8310=ORIENTED_EDGE('',*,*,#6518,.T.);
#8311=ORIENTED_EDGE('',*,*,#6519,.T.);
#8312=ORIENTED_EDGE('',*,*,#6518,.F.);
#8313=ORIENTED_EDGE('',*,*,#6519,.F.);
#8314=ORIENTED_EDGE('',*,*,#6520,.F.);
#8315=ORIENTED_EDGE('',*,*,#6521,.F.);
#8316=ORIENTED_EDGE('',*,*,#6522,.T.);
#8317=ORIENTED_EDGE('',*,*,#6520,.T.);
#8318=ORIENTED_EDGE('',*,*,#6522,.F.);
#8319=ORIENTED_EDGE('',*,*,#6496,.T.);
#8320=ORIENTED_EDGE('',*,*,#6517,.T.);
#8321=ORIENTED_EDGE('',*,*,#6500,.T.);
#8322=ORIENTED_EDGE('',*,*,#6515,.T.);
#8323=ORIENTED_EDGE('',*,*,#6504,.T.);
#8324=ORIENTED_EDGE('',*,*,#6514,.T.);
#8325=ORIENTED_EDGE('',*,*,#6508,.T.);
#8326=ORIENTED_EDGE('',*,*,#6516,.T.);
#8327=ORIENTED_EDGE('',*,*,#6521,.T.);
#8328=ORIENTED_EDGE('',*,*,#6523,.F.);
#8329=ORIENTED_EDGE('',*,*,#6524,.T.);
#8330=ORIENTED_EDGE('',*,*,#6525,.F.);
#8331=ORIENTED_EDGE('',*,*,#6524,.F.);
#8332=ORIENTED_EDGE('',*,*,#6523,.T.);
#8333=ORIENTED_EDGE('',*,*,#6526,.F.);
#8334=ORIENTED_EDGE('',*,*,#6527,.F.);
#8335=ORIENTED_EDGE('',*,*,#6528,.T.);
#8336=ORIENTED_EDGE('',*,*,#6529,.F.);
#8337=ORIENTED_EDGE('',*,*,#6528,.F.);
#8338=ORIENTED_EDGE('',*,*,#6527,.T.);
#8339=ORIENTED_EDGE('',*,*,#6530,.F.);
#8340=ORIENTED_EDGE('',*,*,#6531,.F.);
#8341=ORIENTED_EDGE('',*,*,#6532,.T.);
#8342=ORIENTED_EDGE('',*,*,#6526,.T.);
#8343=ORIENTED_EDGE('',*,*,#6532,.F.);
#8344=ORIENTED_EDGE('',*,*,#6533,.F.);
#8345=ORIENTED_EDGE('',*,*,#6534,.T.);
#8346=ORIENTED_EDGE('',*,*,#6530,.T.);
#8347=ORIENTED_EDGE('',*,*,#6534,.F.);
#8348=ORIENTED_EDGE('',*,*,#6535,.F.);
#8349=ORIENTED_EDGE('',*,*,#6536,.T.);
#8350=ORIENTED_EDGE('',*,*,#6537,.F.);
#8351=ORIENTED_EDGE('',*,*,#6536,.F.);
#8352=ORIENTED_EDGE('',*,*,#6538,.T.);
#8353=ORIENTED_EDGE('',*,*,#6539,.T.);
#8354=ORIENTED_EDGE('',*,*,#6540,.F.);
#8355=ORIENTED_EDGE('',*,*,#6541,.F.);
#8356=ORIENTED_EDGE('',*,*,#6542,.T.);
#8357=ORIENTED_EDGE('',*,*,#6541,.T.);
#8358=ORIENTED_EDGE('',*,*,#6543,.F.);
#8359=ORIENTED_EDGE('',*,*,#6544,.F.);
#8360=ORIENTED_EDGE('',*,*,#6537,.T.);
#8361=ORIENTED_EDGE('',*,*,#6545,.T.);
#8362=ORIENTED_EDGE('',*,*,#6544,.T.);
#8363=ORIENTED_EDGE('',*,*,#6546,.F.);
#8364=ORIENTED_EDGE('',*,*,#6547,.F.);
#8365=ORIENTED_EDGE('',*,*,#6548,.T.);
#8366=ORIENTED_EDGE('',*,*,#6547,.T.);
#8367=ORIENTED_EDGE('',*,*,#6549,.F.);
#8368=ORIENTED_EDGE('',*,*,#6539,.F.);
#8369=ORIENTED_EDGE('',*,*,#6535,.T.);
#8370=ORIENTED_EDGE('',*,*,#6549,.T.);
#8371=ORIENTED_EDGE('',*,*,#6546,.T.);
#8372=ORIENTED_EDGE('',*,*,#6543,.T.);
#8373=ORIENTED_EDGE('',*,*,#6540,.T.);
#8374=ORIENTED_EDGE('',*,*,#6525,.T.);
#8375=ORIENTED_EDGE('',*,*,#6529,.T.);
#8376=ORIENTED_EDGE('',*,*,#6548,.F.);
#8377=ORIENTED_EDGE('',*,*,#6538,.F.);
#8378=ORIENTED_EDGE('',*,*,#6542,.F.);
#8379=ORIENTED_EDGE('',*,*,#6545,.F.);
#8380=ORIENTED_EDGE('',*,*,#6531,.T.);
#8381=ORIENTED_EDGE('',*,*,#6533,.T.);
#8382=ORIENTED_EDGE('',*,*,#6550,.F.);
#8383=ORIENTED_EDGE('',*,*,#6551,.T.);
#8384=ORIENTED_EDGE('',*,*,#6552,.T.);
#8385=ORIENTED_EDGE('',*,*,#6551,.F.);
#8386=ORIENTED_EDGE('',*,*,#6553,.F.);
#8387=ORIENTED_EDGE('',*,*,#6554,.T.);
#8388=ORIENTED_EDGE('',*,*,#6555,.T.);
#8389=ORIENTED_EDGE('',*,*,#6554,.F.);
#8390=ORIENTED_EDGE('',*,*,#6553,.T.);
#8391=ORIENTED_EDGE('',*,*,#6550,.T.);
#8392=ORIENTED_EDGE('',*,*,#6555,.F.);
#8393=ORIENTED_EDGE('',*,*,#6552,.F.);
#8394=ORIENTED_EDGE('',*,*,#6556,.F.);
#8395=ORIENTED_EDGE('',*,*,#6557,.T.);
#8396=ORIENTED_EDGE('',*,*,#6558,.F.);
#8397=ORIENTED_EDGE('',*,*,#6557,.F.);
#8398=ORIENTED_EDGE('',*,*,#6556,.T.);
#8399=ORIENTED_EDGE('',*,*,#6559,.F.);
#8400=ORIENTED_EDGE('',*,*,#6560,.F.);
#8401=ORIENTED_EDGE('',*,*,#6561,.T.);
#8402=ORIENTED_EDGE('',*,*,#6562,.F.);
#8403=ORIENTED_EDGE('',*,*,#6561,.F.);
#8404=ORIENTED_EDGE('',*,*,#6560,.T.);
#8405=ORIENTED_EDGE('',*,*,#6563,.F.);
#8406=ORIENTED_EDGE('',*,*,#6564,.F.);
#8407=ORIENTED_EDGE('',*,*,#6565,.T.);
#8408=ORIENTED_EDGE('',*,*,#6559,.T.);
#8409=ORIENTED_EDGE('',*,*,#6565,.F.);
#8410=ORIENTED_EDGE('',*,*,#6566,.F.);
#8411=ORIENTED_EDGE('',*,*,#6567,.T.);
#8412=ORIENTED_EDGE('',*,*,#6563,.T.);
#8413=ORIENTED_EDGE('',*,*,#6567,.F.);
#8414=ORIENTED_EDGE('',*,*,#6568,.F.);
#8415=ORIENTED_EDGE('',*,*,#6569,.T.);
#8416=ORIENTED_EDGE('',*,*,#6570,.F.);
#8417=ORIENTED_EDGE('',*,*,#6569,.F.);
#8418=ORIENTED_EDGE('',*,*,#6571,.T.);
#8419=ORIENTED_EDGE('',*,*,#6572,.T.);
#8420=ORIENTED_EDGE('',*,*,#6573,.F.);
#8421=ORIENTED_EDGE('',*,*,#6574,.F.);
#8422=ORIENTED_EDGE('',*,*,#6575,.T.);
#8423=ORIENTED_EDGE('',*,*,#6574,.T.);
#8424=ORIENTED_EDGE('',*,*,#6576,.F.);
#8425=ORIENTED_EDGE('',*,*,#6577,.F.);
#8426=ORIENTED_EDGE('',*,*,#6570,.T.);
#8427=ORIENTED_EDGE('',*,*,#6578,.T.);
#8428=ORIENTED_EDGE('',*,*,#6577,.T.);
#8429=ORIENTED_EDGE('',*,*,#6579,.F.);
#8430=ORIENTED_EDGE('',*,*,#6580,.F.);
#8431=ORIENTED_EDGE('',*,*,#6581,.T.);
#8432=ORIENTED_EDGE('',*,*,#6580,.T.);
#8433=ORIENTED_EDGE('',*,*,#6582,.F.);
#8434=ORIENTED_EDGE('',*,*,#6572,.F.);
#8435=ORIENTED_EDGE('',*,*,#6568,.T.);
#8436=ORIENTED_EDGE('',*,*,#6582,.T.);
#8437=ORIENTED_EDGE('',*,*,#6579,.T.);
#8438=ORIENTED_EDGE('',*,*,#6576,.T.);
#8439=ORIENTED_EDGE('',*,*,#6573,.T.);
#8440=ORIENTED_EDGE('',*,*,#6558,.T.);
#8441=ORIENTED_EDGE('',*,*,#6562,.T.);
#8442=ORIENTED_EDGE('',*,*,#6581,.F.);
#8443=ORIENTED_EDGE('',*,*,#6571,.F.);
#8444=ORIENTED_EDGE('',*,*,#6575,.F.);
#8445=ORIENTED_EDGE('',*,*,#6578,.F.);
#8446=ORIENTED_EDGE('',*,*,#6564,.T.);
#8447=ORIENTED_EDGE('',*,*,#6566,.T.);
#8448=ORIENTED_EDGE('',*,*,#6583,.F.);
#8449=ORIENTED_EDGE('',*,*,#6584,.T.);
#8450=ORIENTED_EDGE('',*,*,#6585,.T.);
#8451=ORIENTED_EDGE('',*,*,#6584,.F.);
#8452=ORIENTED_EDGE('',*,*,#6586,.F.);
#8453=ORIENTED_EDGE('',*,*,#6587,.T.);
#8454=ORIENTED_EDGE('',*,*,#6588,.T.);
#8455=ORIENTED_EDGE('',*,*,#6587,.F.);
#8456=ORIENTED_EDGE('',*,*,#6586,.T.);
#8457=ORIENTED_EDGE('',*,*,#6583,.T.);
#8458=ORIENTED_EDGE('',*,*,#6588,.F.);
#8459=ORIENTED_EDGE('',*,*,#6585,.F.);
#8460=ORIENTED_EDGE('',*,*,#6589,.F.);
#8461=ORIENTED_EDGE('',*,*,#6590,.T.);
#8462=ORIENTED_EDGE('',*,*,#6591,.T.);
#8463=ORIENTED_EDGE('',*,*,#6590,.F.);
#8464=ORIENTED_EDGE('',*,*,#6592,.F.);
#8465=ORIENTED_EDGE('',*,*,#6593,.T.);
#8466=ORIENTED_EDGE('',*,*,#6594,.T.);
#8467=ORIENTED_EDGE('',*,*,#6593,.F.);
#8468=ORIENTED_EDGE('',*,*,#6592,.T.);
#8469=ORIENTED_EDGE('',*,*,#6589,.T.);
#8470=ORIENTED_EDGE('',*,*,#6594,.F.);
#8471=ORIENTED_EDGE('',*,*,#6591,.F.);
#8472=ORIENTED_EDGE('',*,*,#6595,.F.);
#8473=ORIENTED_EDGE('',*,*,#6596,.F.);
#8474=ORIENTED_EDGE('',*,*,#6597,.T.);
#8475=ORIENTED_EDGE('',*,*,#6598,.F.);
#8476=ORIENTED_EDGE('',*,*,#6599,.F.);
#8477=ORIENTED_EDGE('',*,*,#6600,.F.);
#8478=ORIENTED_EDGE('',*,*,#6601,.F.);
#8479=ORIENTED_EDGE('',*,*,#6602,.T.);
#8480=ORIENTED_EDGE('',*,*,#6603,.F.);
#8481=ORIENTED_EDGE('',*,*,#6604,.F.);
#8482=ORIENTED_EDGE('',*,*,#6600,.T.);
#8483=ORIENTED_EDGE('',*,*,#6605,.F.);
#8484=ORIENTED_EDGE('',*,*,#6606,.F.);
#8485=ORIENTED_EDGE('',*,*,#6607,.F.);
#8486=ORIENTED_EDGE('',*,*,#6608,.F.);
#8487=ORIENTED_EDGE('',*,*,#6601,.T.);
#8488=ORIENTED_EDGE('',*,*,#6608,.T.);
#8489=ORIENTED_EDGE('',*,*,#6609,.F.);
#8490=ORIENTED_EDGE('',*,*,#6595,.T.);
#8491=ORIENTED_EDGE('',*,*,#6610,.F.);
#8492=ORIENTED_EDGE('',*,*,#6611,.F.);
#8493=ORIENTED_EDGE('',*,*,#6612,.F.);
#8494=ORIENTED_EDGE('',*,*,#6613,.F.);
#8495=ORIENTED_EDGE('',*,*,#6596,.T.);
#8496=ORIENTED_EDGE('',*,*,#6613,.T.);
#8497=ORIENTED_EDGE('',*,*,#6614,.F.);
#8498=ORIENTED_EDGE('',*,*,#6606,.T.);
#8499=ORIENTED_EDGE('',*,*,#6615,.T.);
#8500=ORIENTED_EDGE('',*,*,#6616,.T.);
#8501=ORIENTED_EDGE('',*,*,#6617,.T.);
#8502=ORIENTED_EDGE('',*,*,#6611,.T.);
#8503=ORIENTED_EDGE('',*,*,#6618,.T.);
#8504=ORIENTED_EDGE('',*,*,#6619,.T.);
#8505=ORIENTED_EDGE('',*,*,#6620,.T.);
#8506=ORIENTED_EDGE('',*,*,#6598,.T.);
#8507=ORIENTED_EDGE('',*,*,#6621,.T.);
#8508=ORIENTED_EDGE('',*,*,#6622,.T.);
#8509=ORIENTED_EDGE('',*,*,#6623,.T.);
#8510=ORIENTED_EDGE('',*,*,#6624,.F.);
#8511=ORIENTED_EDGE('',*,*,#6625,.T.);
#8512=ORIENTED_EDGE('',*,*,#6609,.T.);
#8513=ORIENTED_EDGE('',*,*,#6625,.F.);
#8514=ORIENTED_EDGE('',*,*,#6626,.F.);
#8515=ORIENTED_EDGE('',*,*,#6627,.T.);
#8516=ORIENTED_EDGE('',*,*,#6614,.T.);
#8517=ORIENTED_EDGE('',*,*,#6627,.F.);
#8518=ORIENTED_EDGE('',*,*,#6605,.T.);
#8519=ORIENTED_EDGE('',*,*,#6604,.T.);
#8520=ORIENTED_EDGE('',*,*,#6628,.F.);
#8521=ORIENTED_EDGE('',*,*,#6629,.F.);
#8522=ORIENTED_EDGE('',*,*,#6618,.F.);
#8523=ORIENTED_EDGE('',*,*,#6610,.T.);
#8524=ORIENTED_EDGE('',*,*,#6599,.T.);
#8525=ORIENTED_EDGE('',*,*,#6623,.F.);
#8526=ORIENTED_EDGE('',*,*,#6630,.F.);
#8527=ORIENTED_EDGE('',*,*,#6615,.F.);
#8528=ORIENTED_EDGE('',*,*,#6629,.T.);
#8529=ORIENTED_EDGE('',*,*,#6631,.F.);
#8530=ORIENTED_EDGE('',*,*,#6632,.F.);
#8531=ORIENTED_EDGE('',*,*,#6633,.T.);
#8532=ORIENTED_EDGE('',*,*,#6634,.T.);
#8533=ORIENTED_EDGE('',*,*,#6619,.F.);
#8534=ORIENTED_EDGE('',*,*,#6603,.T.);
#8535=ORIENTED_EDGE('',*,*,#6635,.T.);
#8536=ORIENTED_EDGE('',*,*,#6631,.T.);
#8537=ORIENTED_EDGE('',*,*,#6628,.T.);
#8538=ORIENTED_EDGE('',*,*,#6636,.T.);
#8539=ORIENTED_EDGE('',*,*,#6637,.T.);
#8540=ORIENTED_EDGE('',*,*,#6621,.F.);
#8541=ORIENTED_EDGE('',*,*,#6597,.F.);
#8542=ORIENTED_EDGE('',*,*,#6612,.T.);
#8543=ORIENTED_EDGE('',*,*,#6620,.F.);
#8544=ORIENTED_EDGE('',*,*,#6634,.F.);
#8545=ORIENTED_EDGE('',*,*,#6638,.T.);
#8546=ORIENTED_EDGE('',*,*,#6632,.T.);
#8547=ORIENTED_EDGE('',*,*,#6635,.F.);
#8548=ORIENTED_EDGE('',*,*,#6602,.F.);
#8549=ORIENTED_EDGE('',*,*,#6607,.T.);
#8550=ORIENTED_EDGE('',*,*,#6617,.F.);
#8551=ORIENTED_EDGE('',*,*,#6639,.F.);
#8552=ORIENTED_EDGE('',*,*,#6630,.T.);
#8553=ORIENTED_EDGE('',*,*,#6622,.F.);
#8554=ORIENTED_EDGE('',*,*,#6637,.F.);
#8555=ORIENTED_EDGE('',*,*,#6640,.T.);
#8556=ORIENTED_EDGE('',*,*,#6639,.T.);
#8557=ORIENTED_EDGE('',*,*,#6616,.F.);
#8558=ORIENTED_EDGE('',*,*,#6640,.F.);
#8559=ORIENTED_EDGE('',*,*,#6636,.F.);
#8560=ORIENTED_EDGE('',*,*,#6633,.F.);
#8561=ORIENTED_EDGE('',*,*,#6638,.F.);
#8562=ORIENTED_EDGE('',*,*,#6624,.T.);
#8563=ORIENTED_EDGE('',*,*,#6626,.T.);
#8564=ORIENTED_EDGE('',*,*,#6641,.F.);
#8565=ORIENTED_EDGE('',*,*,#6642,.T.);
#8566=ORIENTED_EDGE('',*,*,#6643,.F.);
#8567=ORIENTED_EDGE('',*,*,#6642,.F.);
#8568=ORIENTED_EDGE('',*,*,#6641,.T.);
#8569=ORIENTED_EDGE('',*,*,#6644,.F.);
#8570=ORIENTED_EDGE('',*,*,#6645,.F.);
#8571=ORIENTED_EDGE('',*,*,#6646,.T.);
#8572=ORIENTED_EDGE('',*,*,#6647,.F.);
#8573=ORIENTED_EDGE('',*,*,#6646,.F.);
#8574=ORIENTED_EDGE('',*,*,#6645,.T.);
#8575=ORIENTED_EDGE('',*,*,#6648,.F.);
#8576=ORIENTED_EDGE('',*,*,#6649,.F.);
#8577=ORIENTED_EDGE('',*,*,#6650,.T.);
#8578=ORIENTED_EDGE('',*,*,#6651,.F.);
#8579=ORIENTED_EDGE('',*,*,#6650,.F.);
#8580=ORIENTED_EDGE('',*,*,#6649,.T.);
#8581=ORIENTED_EDGE('',*,*,#6652,.F.);
#8582=ORIENTED_EDGE('',*,*,#6653,.F.);
#8583=ORIENTED_EDGE('',*,*,#6654,.T.);
#8584=ORIENTED_EDGE('',*,*,#6655,.F.);
#8585=ORIENTED_EDGE('',*,*,#6654,.F.);
#8586=ORIENTED_EDGE('',*,*,#6653,.T.);
#8587=ORIENTED_EDGE('',*,*,#6656,.F.);
#8588=ORIENTED_EDGE('',*,*,#6657,.F.);
#8589=ORIENTED_EDGE('',*,*,#6658,.T.);
#8590=ORIENTED_EDGE('',*,*,#6644,.T.);
#8591=ORIENTED_EDGE('',*,*,#6658,.F.);
#8592=ORIENTED_EDGE('',*,*,#6659,.F.);
#8593=ORIENTED_EDGE('',*,*,#6660,.T.);
#8594=ORIENTED_EDGE('',*,*,#6648,.T.);
#8595=ORIENTED_EDGE('',*,*,#6660,.F.);
#8596=ORIENTED_EDGE('',*,*,#6661,.F.);
#8597=ORIENTED_EDGE('',*,*,#6662,.T.);
#8598=ORIENTED_EDGE('',*,*,#6652,.T.);
#8599=ORIENTED_EDGE('',*,*,#6662,.F.);
#8600=ORIENTED_EDGE('',*,*,#6663,.F.);
#8601=ORIENTED_EDGE('',*,*,#6664,.T.);
#8602=ORIENTED_EDGE('',*,*,#6656,.T.);
#8603=ORIENTED_EDGE('',*,*,#6664,.F.);
#8604=ORIENTED_EDGE('',*,*,#6665,.T.);
#8605=ORIENTED_EDGE('',*,*,#6666,.T.);
#8606=ORIENTED_EDGE('',*,*,#6667,.F.);
#8607=ORIENTED_EDGE('',*,*,#6668,.F.);
#8608=ORIENTED_EDGE('',*,*,#6669,.T.);
#8609=ORIENTED_EDGE('',*,*,#6668,.T.);
#8610=ORIENTED_EDGE('',*,*,#6670,.F.);
#8611=ORIENTED_EDGE('',*,*,#6671,.F.);
#8612=ORIENTED_EDGE('',*,*,#6672,.T.);
#8613=ORIENTED_EDGE('',*,*,#6671,.T.);
#8614=ORIENTED_EDGE('',*,*,#6673,.F.);
#8615=ORIENTED_EDGE('',*,*,#6674,.F.);
#8616=ORIENTED_EDGE('',*,*,#6675,.T.);
#8617=ORIENTED_EDGE('',*,*,#6674,.T.);
#8618=ORIENTED_EDGE('',*,*,#6676,.F.);
#8619=ORIENTED_EDGE('',*,*,#6677,.F.);
#8620=ORIENTED_EDGE('',*,*,#6678,.T.);
#8621=ORIENTED_EDGE('',*,*,#6677,.T.);
#8622=ORIENTED_EDGE('',*,*,#6679,.F.);
#8623=ORIENTED_EDGE('',*,*,#6680,.F.);
#8624=ORIENTED_EDGE('',*,*,#6655,.T.);
#8625=ORIENTED_EDGE('',*,*,#6651,.T.);
#8626=ORIENTED_EDGE('',*,*,#6647,.T.);
#8627=ORIENTED_EDGE('',*,*,#6643,.T.);
#8628=ORIENTED_EDGE('',*,*,#6681,.T.);
#8629=ORIENTED_EDGE('',*,*,#6680,.T.);
#8630=ORIENTED_EDGE('',*,*,#6682,.F.);
#8631=ORIENTED_EDGE('',*,*,#6683,.F.);
#8632=ORIENTED_EDGE('',*,*,#6684,.T.);
#8633=ORIENTED_EDGE('',*,*,#6683,.T.);
#8634=ORIENTED_EDGE('',*,*,#6685,.F.);
#8635=ORIENTED_EDGE('',*,*,#6686,.F.);
#8636=ORIENTED_EDGE('',*,*,#6687,.T.);
#8637=ORIENTED_EDGE('',*,*,#6686,.T.);
#8638=ORIENTED_EDGE('',*,*,#6688,.F.);
#8639=ORIENTED_EDGE('',*,*,#6689,.F.);
#8640=ORIENTED_EDGE('',*,*,#6690,.T.);
#8641=ORIENTED_EDGE('',*,*,#6689,.T.);
#8642=ORIENTED_EDGE('',*,*,#6691,.F.);
#8643=ORIENTED_EDGE('',*,*,#6692,.F.);
#8644=ORIENTED_EDGE('',*,*,#6693,.T.);
#8645=ORIENTED_EDGE('',*,*,#6692,.T.);
#8646=ORIENTED_EDGE('',*,*,#6694,.F.);
#8647=ORIENTED_EDGE('',*,*,#6695,.F.);
#8648=ORIENTED_EDGE('',*,*,#6696,.T.);
#8649=ORIENTED_EDGE('',*,*,#6695,.T.);
#8650=ORIENTED_EDGE('',*,*,#6697,.F.);
#8651=ORIENTED_EDGE('',*,*,#6698,.F.);
#8652=ORIENTED_EDGE('',*,*,#6657,.T.);
#8653=ORIENTED_EDGE('',*,*,#6659,.T.);
#8654=ORIENTED_EDGE('',*,*,#6661,.T.);
#8655=ORIENTED_EDGE('',*,*,#6663,.T.);
#8656=ORIENTED_EDGE('',*,*,#6699,.T.);
#8657=ORIENTED_EDGE('',*,*,#6698,.T.);
#8658=ORIENTED_EDGE('',*,*,#6700,.F.);
#8659=ORIENTED_EDGE('',*,*,#6666,.F.);
#8660=ORIENTED_EDGE('',*,*,#6700,.T.);
#8661=ORIENTED_EDGE('',*,*,#6697,.T.);
#8662=ORIENTED_EDGE('',*,*,#6694,.T.);
#8663=ORIENTED_EDGE('',*,*,#6691,.T.);
#8664=ORIENTED_EDGE('',*,*,#6688,.T.);
#8665=ORIENTED_EDGE('',*,*,#6685,.T.);
#8666=ORIENTED_EDGE('',*,*,#6682,.T.);
#8667=ORIENTED_EDGE('',*,*,#6679,.T.);
#8668=ORIENTED_EDGE('',*,*,#6676,.T.);
#8669=ORIENTED_EDGE('',*,*,#6673,.T.);
#8670=ORIENTED_EDGE('',*,*,#6670,.T.);
#8671=ORIENTED_EDGE('',*,*,#6667,.T.);
#8672=ORIENTED_EDGE('',*,*,#6699,.F.);
#8673=ORIENTED_EDGE('',*,*,#6665,.F.);
#8674=ORIENTED_EDGE('',*,*,#6669,.F.);
#8675=ORIENTED_EDGE('',*,*,#6672,.F.);
#8676=ORIENTED_EDGE('',*,*,#6675,.F.);
#8677=ORIENTED_EDGE('',*,*,#6678,.F.);
#8678=ORIENTED_EDGE('',*,*,#6681,.F.);
#8679=ORIENTED_EDGE('',*,*,#6684,.F.);
#8680=ORIENTED_EDGE('',*,*,#6687,.F.);
#8681=ORIENTED_EDGE('',*,*,#6690,.F.);
#8682=ORIENTED_EDGE('',*,*,#6693,.F.);
#8683=ORIENTED_EDGE('',*,*,#6696,.F.);
#8684=ORIENTED_EDGE('',*,*,#6701,.F.);
#8685=ORIENTED_EDGE('',*,*,#6702,.F.);
#8686=ORIENTED_EDGE('',*,*,#6703,.T.);
#8687=ORIENTED_EDGE('',*,*,#6704,.F.);
#8688=ORIENTED_EDGE('',*,*,#6705,.F.);
#8689=ORIENTED_EDGE('',*,*,#6703,.F.);
#8690=ORIENTED_EDGE('',*,*,#6704,.T.);
#8691=ORIENTED_EDGE('',*,*,#6705,.T.);
#8692=ORIENTED_EDGE('',*,*,#6706,.T.);
#8693=ORIENTED_EDGE('',*,*,#6707,.T.);
#8694=ORIENTED_EDGE('',*,*,#6706,.F.);
#8695=ORIENTED_EDGE('',*,*,#6708,.T.);
#8696=ORIENTED_EDGE('',*,*,#6709,.T.);
#8697=ORIENTED_EDGE('',*,*,#6710,.F.);
#8698=ORIENTED_EDGE('',*,*,#6709,.F.);
#8699=ORIENTED_EDGE('',*,*,#6710,.T.);
#8700=ORIENTED_EDGE('',*,*,#6711,.T.);
#8701=ORIENTED_EDGE('',*,*,#6712,.F.);
#8702=ORIENTED_EDGE('',*,*,#6711,.F.);
#8703=ORIENTED_EDGE('',*,*,#6707,.F.);
#8704=ORIENTED_EDGE('',*,*,#6712,.T.);
#8705=ORIENTED_EDGE('',*,*,#6713,.F.);
#8706=ORIENTED_EDGE('',*,*,#6714,.T.);
#8707=ORIENTED_EDGE('',*,*,#6701,.T.);
#8708=ORIENTED_EDGE('',*,*,#6702,.T.);
#8709=ORIENTED_EDGE('',*,*,#6714,.F.);
#8710=ORIENTED_EDGE('',*,*,#6713,.T.);
#8711=ORIENTED_EDGE('',*,*,#6715,.F.);
#8712=ORIENTED_EDGE('',*,*,#6715,.T.);
#8713=ORIENTED_EDGE('',*,*,#6716,.T.);
#8714=ORIENTED_EDGE('',*,*,#6708,.F.);
#8715=ORIENTED_EDGE('',*,*,#6716,.F.);
#8716=ORIENTED_EDGE('',*,*,#6717,.F.);
#8717=ORIENTED_EDGE('',*,*,#6718,.F.);
#8718=ORIENTED_EDGE('',*,*,#6719,.T.);
#8719=ORIENTED_EDGE('',*,*,#6720,.F.);
#8720=ORIENTED_EDGE('',*,*,#6721,.F.);
#8721=ORIENTED_EDGE('',*,*,#6719,.F.);
#8722=ORIENTED_EDGE('',*,*,#6722,.T.);
#8723=ORIENTED_EDGE('',*,*,#6723,.T.);
#8724=ORIENTED_EDGE('',*,*,#6720,.T.);
#8725=ORIENTED_EDGE('',*,*,#6721,.T.);
#8726=ORIENTED_EDGE('',*,*,#6723,.F.);
#8727=ORIENTED_EDGE('',*,*,#6724,.F.);
#8728=ORIENTED_EDGE('',*,*,#6725,.T.);
#8729=ORIENTED_EDGE('',*,*,#6726,.F.);
#8730=ORIENTED_EDGE('',*,*,#6727,.T.);
#8731=ORIENTED_EDGE('',*,*,#6724,.T.);
#8732=ORIENTED_EDGE('',*,*,#6727,.F.);
#8733=ORIENTED_EDGE('',*,*,#6728,.F.);
#8734=ORIENTED_EDGE('',*,*,#6729,.T.);
#8735=ORIENTED_EDGE('',*,*,#6726,.T.);
#8736=ORIENTED_EDGE('',*,*,#6729,.F.);
#8737=ORIENTED_EDGE('',*,*,#6730,.F.);
#8738=ORIENTED_EDGE('',*,*,#6731,.T.);
#8739=ORIENTED_EDGE('',*,*,#6728,.T.);
#8740=ORIENTED_EDGE('',*,*,#6731,.F.);
#8741=ORIENTED_EDGE('',*,*,#6730,.T.);
#8742=ORIENTED_EDGE('',*,*,#6722,.F.);
#8743=ORIENTED_EDGE('',*,*,#6717,.T.);
#8744=ORIENTED_EDGE('',*,*,#6718,.T.);
#8745=ORIENTED_EDGE('',*,*,#6732,.T.);
#8746=ORIENTED_EDGE('',*,*,#6725,.F.);
#8747=ORIENTED_EDGE('',*,*,#6732,.F.);
#8748=ORIENTED_EDGE('',*,*,#6733,.T.);
#8749=ORIENTED_EDGE('',*,*,#6733,.F.);
#8750=ORIENTED_EDGE('',*,*,#6734,.T.);
#8751=ORIENTED_EDGE('',*,*,#6734,.F.);
#8752=ORIENTED_EDGE('',*,*,#6735,.T.);
#8753=ORIENTED_EDGE('',*,*,#6735,.F.);
#8754=ORIENTED_EDGE('',*,*,#6736,.T.);
#8755=ORIENTED_EDGE('',*,*,#6736,.F.);
#8756=ORIENTED_EDGE('',*,*,#6737,.T.);
#8757=ORIENTED_EDGE('',*,*,#6737,.F.);
#8758=ORIENTED_EDGE('',*,*,#6738,.T.);
#8759=ORIENTED_EDGE('',*,*,#6738,.F.);
#8760=ORIENTED_EDGE('',*,*,#6739,.T.);
#8761=ORIENTED_EDGE('',*,*,#6739,.F.);
#8762=ORIENTED_EDGE('',*,*,#6740,.T.);
#8763=ORIENTED_EDGE('',*,*,#6740,.F.);
#8764=ORIENTED_EDGE('',*,*,#6741,.F.);
#8765=ORIENTED_EDGE('',*,*,#6742,.F.);
#8766=ORIENTED_EDGE('',*,*,#6743,.F.);
#8767=ORIENTED_EDGE('',*,*,#6744,.F.);
#8768=ORIENTED_EDGE('',*,*,#6743,.T.);
#8769=ORIENTED_EDGE('',*,*,#6745,.F.);
#8770=ORIENTED_EDGE('',*,*,#6746,.T.);
#8771=ORIENTED_EDGE('',*,*,#6747,.F.);
#8772=ORIENTED_EDGE('',*,*,#6748,.T.);
#8773=ORIENTED_EDGE('',*,*,#6749,.F.);
#8774=ORIENTED_EDGE('',*,*,#6750,.T.);
#8775=ORIENTED_EDGE('',*,*,#6751,.T.);
#8776=ORIENTED_EDGE('',*,*,#6752,.F.);
#8777=ORIENTED_EDGE('',*,*,#6751,.F.);
#8778=ORIENTED_EDGE('',*,*,#6753,.T.);
#8779=ORIENTED_EDGE('',*,*,#6754,.F.);
#8780=ORIENTED_EDGE('',*,*,#6755,.T.);
#8781=ORIENTED_EDGE('',*,*,#6756,.F.);
#8782=ORIENTED_EDGE('',*,*,#6757,.T.);
#8783=ORIENTED_EDGE('',*,*,#6758,.F.);
#8784=ORIENTED_EDGE('',*,*,#6759,.T.);
#8785=ORIENTED_EDGE('',*,*,#6760,.F.);
#8786=ORIENTED_EDGE('',*,*,#6761,.T.);
#8787=ORIENTED_EDGE('',*,*,#6762,.F.);
#8788=ORIENTED_EDGE('',*,*,#6742,.T.);
#8789=ORIENTED_EDGE('',*,*,#6763,.T.);
#8790=ORIENTED_EDGE('',*,*,#6764,.T.);
#8791=ORIENTED_EDGE('',*,*,#6745,.T.);
#8792=ORIENTED_EDGE('',*,*,#6765,.F.);
#8793=ORIENTED_EDGE('',*,*,#6766,.F.);
#8794=ORIENTED_EDGE('',*,*,#6746,.F.);
#8795=ORIENTED_EDGE('',*,*,#6764,.F.);
#8796=ORIENTED_EDGE('',*,*,#6766,.T.);
#8797=ORIENTED_EDGE('',*,*,#6767,.T.);
#8798=ORIENTED_EDGE('',*,*,#6768,.T.);
#8799=ORIENTED_EDGE('',*,*,#6747,.T.);
#8800=ORIENTED_EDGE('',*,*,#6769,.F.);
#8801=ORIENTED_EDGE('',*,*,#6770,.F.);
#8802=ORIENTED_EDGE('',*,*,#6748,.F.);
#8803=ORIENTED_EDGE('',*,*,#6768,.F.);
#8804=ORIENTED_EDGE('',*,*,#6770,.T.);
#8805=ORIENTED_EDGE('',*,*,#6771,.T.);
#8806=ORIENTED_EDGE('',*,*,#6772,.T.);
#8807=ORIENTED_EDGE('',*,*,#6749,.T.);
#8808=ORIENTED_EDGE('',*,*,#6773,.F.);
#8809=ORIENTED_EDGE('',*,*,#6774,.F.);
#8810=ORIENTED_EDGE('',*,*,#6753,.F.);
#8811=ORIENTED_EDGE('',*,*,#6750,.F.);
#8812=ORIENTED_EDGE('',*,*,#6772,.F.);
#8813=ORIENTED_EDGE('',*,*,#6775,.F.);
#8814=ORIENTED_EDGE('',*,*,#6774,.T.);
#8815=ORIENTED_EDGE('',*,*,#6776,.T.);
#8816=ORIENTED_EDGE('',*,*,#6777,.T.);
#8817=ORIENTED_EDGE('',*,*,#6754,.T.);
#8818=ORIENTED_EDGE('',*,*,#6778,.F.);
#8819=ORIENTED_EDGE('',*,*,#6779,.F.);
#8820=ORIENTED_EDGE('',*,*,#6755,.F.);
#8821=ORIENTED_EDGE('',*,*,#6777,.F.);
#8822=ORIENTED_EDGE('',*,*,#6779,.T.);
#8823=ORIENTED_EDGE('',*,*,#6780,.T.);
#8824=ORIENTED_EDGE('',*,*,#6781,.T.);
#8825=ORIENTED_EDGE('',*,*,#6756,.T.);
#8826=ORIENTED_EDGE('',*,*,#6782,.F.);
#8827=ORIENTED_EDGE('',*,*,#6783,.F.);
#8828=ORIENTED_EDGE('',*,*,#6757,.F.);
#8829=ORIENTED_EDGE('',*,*,#6781,.F.);
#8830=ORIENTED_EDGE('',*,*,#6783,.T.);
#8831=ORIENTED_EDGE('',*,*,#6784,.T.);
#8832=ORIENTED_EDGE('',*,*,#6785,.T.);
#8833=ORIENTED_EDGE('',*,*,#6758,.T.);
#8834=ORIENTED_EDGE('',*,*,#6759,.F.);
#8835=ORIENTED_EDGE('',*,*,#6785,.F.);
#8836=ORIENTED_EDGE('',*,*,#6786,.F.);
#8837=ORIENTED_EDGE('',*,*,#6787,.F.);
#8838=ORIENTED_EDGE('',*,*,#6788,.F.);
#8839=ORIENTED_EDGE('',*,*,#6789,.T.);
#8840=ORIENTED_EDGE('',*,*,#6775,.T.);
#8841=ORIENTED_EDGE('',*,*,#6771,.F.);
#8842=ORIENTED_EDGE('',*,*,#6769,.T.);
#8843=ORIENTED_EDGE('',*,*,#6767,.F.);
#8844=ORIENTED_EDGE('',*,*,#6765,.T.);
#8845=ORIENTED_EDGE('',*,*,#6763,.F.);
#8846=ORIENTED_EDGE('',*,*,#6741,.T.);
#8847=ORIENTED_EDGE('',*,*,#6790,.F.);
#8848=ORIENTED_EDGE('',*,*,#6791,.T.);
#8849=ORIENTED_EDGE('',*,*,#6792,.F.);
#8850=ORIENTED_EDGE('',*,*,#6786,.T.);
#8851=ORIENTED_EDGE('',*,*,#6784,.F.);
#8852=ORIENTED_EDGE('',*,*,#6782,.T.);
#8853=ORIENTED_EDGE('',*,*,#6780,.F.);
#8854=ORIENTED_EDGE('',*,*,#6778,.T.);
#8855=ORIENTED_EDGE('',*,*,#6776,.F.);
#8856=ORIENTED_EDGE('',*,*,#6773,.T.);
#8857=ORIENTED_EDGE('',*,*,#6789,.F.);
#8858=ORIENTED_EDGE('',*,*,#6744,.T.);
#8859=ORIENTED_EDGE('',*,*,#6762,.T.);
#8860=ORIENTED_EDGE('',*,*,#6793,.T.);
#8861=ORIENTED_EDGE('',*,*,#6790,.T.);
#8862=ORIENTED_EDGE('',*,*,#6761,.F.);
#8863=ORIENTED_EDGE('',*,*,#6794,.F.);
#8864=ORIENTED_EDGE('',*,*,#6791,.F.);
#8865=ORIENTED_EDGE('',*,*,#6793,.F.);
#8866=ORIENTED_EDGE('',*,*,#6752,.T.);
#8867=ORIENTED_EDGE('',*,*,#6788,.T.);
#8868=ORIENTED_EDGE('',*,*,#6787,.T.);
#8869=ORIENTED_EDGE('',*,*,#6792,.T.);
#8870=ORIENTED_EDGE('',*,*,#6794,.T.);
#8871=ORIENTED_EDGE('',*,*,#6760,.T.);
#8872=ORIENTED_EDGE('',*,*,#6795,.F.);
#8873=ORIENTED_EDGE('',*,*,#6796,.T.);
#8874=ORIENTED_EDGE('',*,*,#6797,.F.);
#8875=ORIENTED_EDGE('',*,*,#6798,.T.);
#8876=ORIENTED_EDGE('',*,*,#6795,.T.);
#8877=ORIENTED_EDGE('',*,*,#6798,.F.);
#8878=ORIENTED_EDGE('',*,*,#6797,.T.);
#8879=ORIENTED_EDGE('',*,*,#6799,.F.);
#8880=ORIENTED_EDGE('',*,*,#6799,.T.);
#8881=ORIENTED_EDGE('',*,*,#6800,.T.);
#8882=ORIENTED_EDGE('',*,*,#6796,.F.);
#8883=ORIENTED_EDGE('',*,*,#6800,.F.);
#8884=ORIENTED_EDGE('',*,*,#6801,.F.);
#8885=ORIENTED_EDGE('',*,*,#6802,.T.);
#8886=ORIENTED_EDGE('',*,*,#6803,.F.);
#8887=ORIENTED_EDGE('',*,*,#6804,.T.);
#8888=ORIENTED_EDGE('',*,*,#6801,.T.);
#8889=ORIENTED_EDGE('',*,*,#6804,.F.);
#8890=ORIENTED_EDGE('',*,*,#6803,.T.);
#8891=ORIENTED_EDGE('',*,*,#6805,.F.);
#8892=ORIENTED_EDGE('',*,*,#6805,.T.);
#8893=ORIENTED_EDGE('',*,*,#6806,.T.);
#8894=ORIENTED_EDGE('',*,*,#6802,.F.);
#8895=ORIENTED_EDGE('',*,*,#6806,.F.);
#8896=ORIENTED_EDGE('',*,*,#6807,.F.);
#8897=ORIENTED_EDGE('',*,*,#6808,.T.);
#8898=ORIENTED_EDGE('',*,*,#6809,.F.);
#8899=ORIENTED_EDGE('',*,*,#6808,.F.);
#8900=ORIENTED_EDGE('',*,*,#6810,.F.);
#8901=ORIENTED_EDGE('',*,*,#6811,.T.);
#8902=ORIENTED_EDGE('',*,*,#6812,.F.);
#8903=ORIENTED_EDGE('',*,*,#6811,.F.);
#8904=ORIENTED_EDGE('',*,*,#6813,.F.);
#8905=ORIENTED_EDGE('',*,*,#6814,.T.);
#8906=ORIENTED_EDGE('',*,*,#6815,.F.);
#8907=ORIENTED_EDGE('',*,*,#6814,.F.);
#8908=ORIENTED_EDGE('',*,*,#6816,.F.);
#8909=ORIENTED_EDGE('',*,*,#6817,.T.);
#8910=ORIENTED_EDGE('',*,*,#6818,.F.);
#8911=ORIENTED_EDGE('',*,*,#6817,.F.);
#8912=ORIENTED_EDGE('',*,*,#6819,.F.);
#8913=ORIENTED_EDGE('',*,*,#6820,.T.);
#8914=ORIENTED_EDGE('',*,*,#6821,.F.);
#8915=ORIENTED_EDGE('',*,*,#6820,.F.);
#8916=ORIENTED_EDGE('',*,*,#6822,.F.);
#8917=ORIENTED_EDGE('',*,*,#6823,.T.);
#8918=ORIENTED_EDGE('',*,*,#6824,.F.);
#8919=ORIENTED_EDGE('',*,*,#6823,.F.);
#8920=ORIENTED_EDGE('',*,*,#6825,.F.);
#8921=ORIENTED_EDGE('',*,*,#6826,.T.);
#8922=ORIENTED_EDGE('',*,*,#6827,.F.);
#8923=ORIENTED_EDGE('',*,*,#6826,.F.);
#8924=ORIENTED_EDGE('',*,*,#6828,.F.);
#8925=ORIENTED_EDGE('',*,*,#6829,.T.);
#8926=ORIENTED_EDGE('',*,*,#6830,.F.);
#8927=ORIENTED_EDGE('',*,*,#6829,.F.);
#8928=ORIENTED_EDGE('',*,*,#6831,.F.);
#8929=ORIENTED_EDGE('',*,*,#6832,.T.);
#8930=ORIENTED_EDGE('',*,*,#6833,.F.);
#8931=ORIENTED_EDGE('',*,*,#6832,.F.);
#8932=ORIENTED_EDGE('',*,*,#6834,.F.);
#8933=ORIENTED_EDGE('',*,*,#6835,.T.);
#8934=ORIENTED_EDGE('',*,*,#6836,.F.);
#8935=ORIENTED_EDGE('',*,*,#6835,.F.);
#8936=ORIENTED_EDGE('',*,*,#6837,.T.);
#8937=ORIENTED_EDGE('',*,*,#6838,.T.);
#8938=ORIENTED_EDGE('',*,*,#6839,.F.);
#8939=ORIENTED_EDGE('',*,*,#6840,.F.);
#8940=ORIENTED_EDGE('',*,*,#6841,.T.);
#8941=ORIENTED_EDGE('',*,*,#6840,.T.);
#8942=ORIENTED_EDGE('',*,*,#6842,.F.);
#8943=ORIENTED_EDGE('',*,*,#6843,.F.);
#8944=ORIENTED_EDGE('',*,*,#6844,.T.);
#8945=ORIENTED_EDGE('',*,*,#6843,.T.);
#8946=ORIENTED_EDGE('',*,*,#6845,.F.);
#8947=ORIENTED_EDGE('',*,*,#6846,.F.);
#8948=ORIENTED_EDGE('',*,*,#6847,.T.);
#8949=ORIENTED_EDGE('',*,*,#6846,.T.);
#8950=ORIENTED_EDGE('',*,*,#6848,.F.);
#8951=ORIENTED_EDGE('',*,*,#6838,.F.);
#8952=ORIENTED_EDGE('',*,*,#6848,.T.);
#8953=ORIENTED_EDGE('',*,*,#6845,.T.);
#8954=ORIENTED_EDGE('',*,*,#6842,.T.);
#8955=ORIENTED_EDGE('',*,*,#6839,.T.);
#8956=ORIENTED_EDGE('',*,*,#6812,.T.);
#8957=ORIENTED_EDGE('',*,*,#6836,.T.);
#8958=ORIENTED_EDGE('',*,*,#6833,.T.);
#8959=ORIENTED_EDGE('',*,*,#6830,.T.);
#8960=ORIENTED_EDGE('',*,*,#6827,.T.);
#8961=ORIENTED_EDGE('',*,*,#6824,.T.);
#8962=ORIENTED_EDGE('',*,*,#6821,.T.);
#8963=ORIENTED_EDGE('',*,*,#6818,.T.);
#8964=ORIENTED_EDGE('',*,*,#6815,.T.);
#8965=ORIENTED_EDGE('',*,*,#6809,.T.);
#8966=ORIENTED_EDGE('',*,*,#6847,.F.);
#8967=ORIENTED_EDGE('',*,*,#6837,.F.);
#8968=ORIENTED_EDGE('',*,*,#6841,.F.);
#8969=ORIENTED_EDGE('',*,*,#6844,.F.);
#8970=ORIENTED_EDGE('',*,*,#6810,.T.);
#8971=ORIENTED_EDGE('',*,*,#6834,.T.);
#8972=ORIENTED_EDGE('',*,*,#6831,.T.);
#8973=ORIENTED_EDGE('',*,*,#6828,.T.);
#8974=ORIENTED_EDGE('',*,*,#6825,.T.);
#8975=ORIENTED_EDGE('',*,*,#6822,.T.);
#8976=ORIENTED_EDGE('',*,*,#6819,.T.);
#8977=ORIENTED_EDGE('',*,*,#6816,.T.);
#8978=ORIENTED_EDGE('',*,*,#6813,.T.);
#8979=ORIENTED_EDGE('',*,*,#6807,.T.);
#8980=ORIENTED_EDGE('',*,*,#6849,.F.);
#8981=ORIENTED_EDGE('',*,*,#6850,.T.);
#8982=ORIENTED_EDGE('',*,*,#6851,.F.);
#8983=ORIENTED_EDGE('',*,*,#6850,.F.);
#8984=ORIENTED_EDGE('',*,*,#6852,.F.);
#8985=ORIENTED_EDGE('',*,*,#6853,.T.);
#8986=ORIENTED_EDGE('',*,*,#6854,.F.);
#8987=ORIENTED_EDGE('',*,*,#6853,.F.);
#8988=ORIENTED_EDGE('',*,*,#6855,.F.);
#8989=ORIENTED_EDGE('',*,*,#6856,.T.);
#8990=ORIENTED_EDGE('',*,*,#6857,.F.);
#8991=ORIENTED_EDGE('',*,*,#6856,.F.);
#8992=ORIENTED_EDGE('',*,*,#6858,.F.);
#8993=ORIENTED_EDGE('',*,*,#6859,.T.);
#8994=ORIENTED_EDGE('',*,*,#6860,.F.);
#8995=ORIENTED_EDGE('',*,*,#6859,.F.);
#8996=ORIENTED_EDGE('',*,*,#6861,.F.);
#8997=ORIENTED_EDGE('',*,*,#6862,.T.);
#8998=ORIENTED_EDGE('',*,*,#6863,.F.);
#8999=ORIENTED_EDGE('',*,*,#6862,.F.);
#9000=ORIENTED_EDGE('',*,*,#6864,.F.);
#9001=ORIENTED_EDGE('',*,*,#6865,.F.);
#9002=ORIENTED_EDGE('',*,*,#6866,.F.);
#9003=ORIENTED_EDGE('',*,*,#6867,.F.);
#9004=ORIENTED_EDGE('',*,*,#6868,.F.);
#9005=ORIENTED_EDGE('',*,*,#6865,.T.);
#9006=ORIENTED_EDGE('',*,*,#6869,.F.);
#9007=ORIENTED_EDGE('',*,*,#6870,.F.);
#9008=ORIENTED_EDGE('',*,*,#6871,.F.);
#9009=ORIENTED_EDGE('',*,*,#6872,.F.);
#9010=ORIENTED_EDGE('',*,*,#6873,.F.);
#9011=ORIENTED_EDGE('',*,*,#6870,.T.);
#9012=ORIENTED_EDGE('',*,*,#6874,.F.);
#9013=ORIENTED_EDGE('',*,*,#6875,.F.);
#9014=ORIENTED_EDGE('',*,*,#6876,.F.);
#9015=ORIENTED_EDGE('',*,*,#6877,.F.);
#9016=ORIENTED_EDGE('',*,*,#6878,.F.);
#9017=ORIENTED_EDGE('',*,*,#6875,.T.);
#9018=ORIENTED_EDGE('',*,*,#6879,.F.);
#9019=ORIENTED_EDGE('',*,*,#6880,.F.);
#9020=ORIENTED_EDGE('',*,*,#6881,.F.);
#9021=ORIENTED_EDGE('',*,*,#6882,.F.);
#9022=ORIENTED_EDGE('',*,*,#6883,.F.);
#9023=ORIENTED_EDGE('',*,*,#6880,.T.);
#9024=ORIENTED_EDGE('',*,*,#6866,.T.);
#9025=ORIENTED_EDGE('',*,*,#6864,.T.);
#9026=ORIENTED_EDGE('',*,*,#6868,.T.);
#9027=ORIENTED_EDGE('',*,*,#6884,.T.);
#9028=ORIENTED_EDGE('',*,*,#6885,.T.);
#9029=ORIENTED_EDGE('',*,*,#6886,.T.);
#9030=ORIENTED_EDGE('',*,*,#6887,.T.);
#9031=ORIENTED_EDGE('',*,*,#6888,.F.);
#9032=ORIENTED_EDGE('',*,*,#6889,.F.);
#9033=ORIENTED_EDGE('',*,*,#6890,.T.);
#9034=ORIENTED_EDGE('',*,*,#6891,.T.);
#9035=ORIENTED_EDGE('',*,*,#6892,.T.);
#9036=ORIENTED_EDGE('',*,*,#6876,.T.);
#9037=ORIENTED_EDGE('',*,*,#6874,.T.);
#9038=ORIENTED_EDGE('',*,*,#6878,.T.);
#9039=ORIENTED_EDGE('',*,*,#6893,.T.);
#9040=ORIENTED_EDGE('',*,*,#6861,.T.);
#9041=ORIENTED_EDGE('',*,*,#6858,.T.);
#9042=ORIENTED_EDGE('',*,*,#6855,.T.);
#9043=ORIENTED_EDGE('',*,*,#6852,.T.);
#9044=ORIENTED_EDGE('',*,*,#6849,.T.);
#9045=ORIENTED_EDGE('',*,*,#6871,.T.);
#9046=ORIENTED_EDGE('',*,*,#6869,.T.);
#9047=ORIENTED_EDGE('',*,*,#6873,.T.);
#9048=ORIENTED_EDGE('',*,*,#6894,.T.);
#9049=ORIENTED_EDGE('',*,*,#6895,.T.);
#9050=ORIENTED_EDGE('',*,*,#6896,.T.);
#9051=ORIENTED_EDGE('',*,*,#6897,.T.);
#9052=ORIENTED_EDGE('',*,*,#6898,.F.);
#9053=ORIENTED_EDGE('',*,*,#6899,.F.);
#9054=ORIENTED_EDGE('',*,*,#6900,.T.);
#9055=ORIENTED_EDGE('',*,*,#6901,.T.);
#9056=ORIENTED_EDGE('',*,*,#6902,.T.);
#9057=ORIENTED_EDGE('',*,*,#6881,.T.);
#9058=ORIENTED_EDGE('',*,*,#6879,.T.);
#9059=ORIENTED_EDGE('',*,*,#6883,.T.);
#9060=ORIENTED_EDGE('',*,*,#6903,.T.);
#9061=ORIENTED_EDGE('',*,*,#6863,.T.);
#9062=ORIENTED_EDGE('',*,*,#6860,.T.);
#9063=ORIENTED_EDGE('',*,*,#6857,.T.);
#9064=ORIENTED_EDGE('',*,*,#6854,.T.);
#9065=ORIENTED_EDGE('',*,*,#6851,.T.);
#9066=ORIENTED_EDGE('',*,*,#6904,.F.);
#9067=ORIENTED_EDGE('',*,*,#6905,.T.);
#9068=ORIENTED_EDGE('',*,*,#6906,.F.);
#9069=ORIENTED_EDGE('',*,*,#6905,.F.);
#9070=ORIENTED_EDGE('',*,*,#6907,.F.);
#9071=ORIENTED_EDGE('',*,*,#6908,.T.);
#9072=ORIENTED_EDGE('',*,*,#6909,.F.);
#9073=ORIENTED_EDGE('',*,*,#6908,.F.);
#9074=ORIENTED_EDGE('',*,*,#6910,.F.);
#9075=ORIENTED_EDGE('',*,*,#6911,.T.);
#9076=ORIENTED_EDGE('',*,*,#6912,.F.);
#9077=ORIENTED_EDGE('',*,*,#6911,.F.);
#9078=ORIENTED_EDGE('',*,*,#6913,.F.);
#9079=ORIENTED_EDGE('',*,*,#6914,.T.);
#9080=ORIENTED_EDGE('',*,*,#6915,.F.);
#9081=ORIENTED_EDGE('',*,*,#6914,.F.);
#9082=ORIENTED_EDGE('',*,*,#6916,.F.);
#9083=ORIENTED_EDGE('',*,*,#6886,.F.);
#9084=ORIENTED_EDGE('',*,*,#6917,.T.);
#9085=ORIENTED_EDGE('',*,*,#6900,.F.);
#9086=ORIENTED_EDGE('',*,*,#6906,.T.);
#9087=ORIENTED_EDGE('',*,*,#6915,.T.);
#9088=ORIENTED_EDGE('',*,*,#6918,.F.);
#9089=ORIENTED_EDGE('',*,*,#6896,.F.);
#9090=ORIENTED_EDGE('',*,*,#6919,.F.);
#9091=ORIENTED_EDGE('',*,*,#6890,.F.);
#9092=ORIENTED_EDGE('',*,*,#6909,.T.);
#9093=ORIENTED_EDGE('',*,*,#6912,.T.);
#9094=ORIENTED_EDGE('',*,*,#6891,.F.);
#9095=ORIENTED_EDGE('',*,*,#6919,.T.);
#9096=ORIENTED_EDGE('',*,*,#6895,.F.);
#9097=ORIENTED_EDGE('',*,*,#6920,.F.);
#9098=ORIENTED_EDGE('',*,*,#6885,.F.);
#9099=ORIENTED_EDGE('',*,*,#6921,.T.);
#9100=ORIENTED_EDGE('',*,*,#6901,.F.);
#9101=ORIENTED_EDGE('',*,*,#6917,.F.);
#9102=ORIENTED_EDGE('',*,*,#6916,.T.);
#9103=ORIENTED_EDGE('',*,*,#6899,.T.);
#9104=ORIENTED_EDGE('',*,*,#6922,.F.);
#9105=ORIENTED_EDGE('',*,*,#6887,.F.);
#9106=ORIENTED_EDGE('',*,*,#6918,.T.);
#9107=ORIENTED_EDGE('',*,*,#6889,.T.);
#9108=ORIENTED_EDGE('',*,*,#6923,.F.);
#9109=ORIENTED_EDGE('',*,*,#6897,.F.);
#9110=ORIENTED_EDGE('',*,*,#6923,.T.);
#9111=ORIENTED_EDGE('',*,*,#6888,.T.);
#9112=ORIENTED_EDGE('',*,*,#6922,.T.);
#9113=ORIENTED_EDGE('',*,*,#6898,.T.);
#9114=ORIENTED_EDGE('',*,*,#6867,.T.);
#9115=ORIENTED_EDGE('',*,*,#6893,.F.);
#9116=ORIENTED_EDGE('',*,*,#6877,.T.);
#9117=ORIENTED_EDGE('',*,*,#6892,.F.);
#9118=ORIENTED_EDGE('',*,*,#6920,.T.);
#9119=ORIENTED_EDGE('',*,*,#6894,.F.);
#9120=ORIENTED_EDGE('',*,*,#6872,.T.);
#9121=ORIENTED_EDGE('',*,*,#6903,.F.);
#9122=ORIENTED_EDGE('',*,*,#6882,.T.);
#9123=ORIENTED_EDGE('',*,*,#6902,.F.);
#9124=ORIENTED_EDGE('',*,*,#6921,.F.);
#9125=ORIENTED_EDGE('',*,*,#6884,.F.);
#9126=ORIENTED_EDGE('',*,*,#6904,.T.);
#9127=ORIENTED_EDGE('',*,*,#6907,.T.);
#9128=ORIENTED_EDGE('',*,*,#6910,.T.);
#9129=ORIENTED_EDGE('',*,*,#6913,.T.);
#9130=ORIENTED_EDGE('',*,*,#6924,.F.);
#9131=ORIENTED_EDGE('',*,*,#6925,.T.);
#9132=ORIENTED_EDGE('',*,*,#6926,.T.);
#9133=ORIENTED_EDGE('',*,*,#6925,.F.);
#9134=ORIENTED_EDGE('',*,*,#6927,.F.);
#9135=ORIENTED_EDGE('',*,*,#6928,.T.);
#9136=ORIENTED_EDGE('',*,*,#6929,.T.);
#9137=ORIENTED_EDGE('',*,*,#6928,.F.);
#9138=ORIENTED_EDGE('',*,*,#6927,.T.);
#9139=ORIENTED_EDGE('',*,*,#6924,.T.);
#9140=ORIENTED_EDGE('',*,*,#6929,.F.);
#9141=ORIENTED_EDGE('',*,*,#6926,.F.);
#9142=ORIENTED_EDGE('',*,*,#6930,.F.);
#9143=ORIENTED_EDGE('',*,*,#6931,.F.);
#9144=ORIENTED_EDGE('',*,*,#6932,.F.);
#9145=ORIENTED_EDGE('',*,*,#6933,.F.);
#9146=ORIENTED_EDGE('',*,*,#6934,.F.);
#9147=ORIENTED_EDGE('',*,*,#6935,.F.);
#9148=ORIENTED_EDGE('',*,*,#6936,.F.);
#9149=ORIENTED_EDGE('',*,*,#6937,.F.);
#9150=ORIENTED_EDGE('',*,*,#6938,.F.);
#9151=ORIENTED_EDGE('',*,*,#6939,.F.);
#9152=ORIENTED_EDGE('',*,*,#6940,.F.);
#9153=ORIENTED_EDGE('',*,*,#6941,.F.);
#9154=ORIENTED_EDGE('',*,*,#6942,.F.);
#9155=ORIENTED_EDGE('',*,*,#6943,.F.);
#9156=ORIENTED_EDGE('',*,*,#6944,.F.);
#9157=ORIENTED_EDGE('',*,*,#6945,.F.);
#9158=ORIENTED_EDGE('',*,*,#6931,.T.);
#9159=ORIENTED_EDGE('',*,*,#6946,.F.);
#9160=ORIENTED_EDGE('',*,*,#6943,.T.);
#9161=ORIENTED_EDGE('',*,*,#6947,.F.);
#9162=ORIENTED_EDGE('',*,*,#6939,.T.);
#9163=ORIENTED_EDGE('',*,*,#6948,.F.);
#9164=ORIENTED_EDGE('',*,*,#6935,.T.);
#9165=ORIENTED_EDGE('',*,*,#6949,.F.);
#9166=ORIENTED_EDGE('',*,*,#6950,.F.);
#9167=ORIENTED_EDGE('',*,*,#6940,.T.);
#9168=ORIENTED_EDGE('',*,*,#6947,.T.);
#9169=ORIENTED_EDGE('',*,*,#6942,.T.);
#9170=ORIENTED_EDGE('',*,*,#6951,.F.);
#9171=ORIENTED_EDGE('',*,*,#6936,.T.);
#9172=ORIENTED_EDGE('',*,*,#6948,.T.);
#9173=ORIENTED_EDGE('',*,*,#6938,.T.);
#9174=ORIENTED_EDGE('',*,*,#6952,.F.);
#9175=ORIENTED_EDGE('',*,*,#6930,.T.);
#9176=ORIENTED_EDGE('',*,*,#6953,.F.);
#9177=ORIENTED_EDGE('',*,*,#6944,.T.);
#9178=ORIENTED_EDGE('',*,*,#6946,.T.);
#9179=ORIENTED_EDGE('',*,*,#6932,.T.);
#9180=ORIENTED_EDGE('',*,*,#6949,.T.);
#9181=ORIENTED_EDGE('',*,*,#6934,.T.);
#9182=ORIENTED_EDGE('',*,*,#6954,.F.);
#9183=ORIENTED_EDGE('',*,*,#6955,.F.);
#9184=ORIENTED_EDGE('',*,*,#6956,.T.);
#9185=ORIENTED_EDGE('',*,*,#6957,.F.);
#9186=ORIENTED_EDGE('',*,*,#6956,.F.);
#9187=ORIENTED_EDGE('',*,*,#6955,.T.);
#9188=ORIENTED_EDGE('',*,*,#6958,.T.);
#9189=ORIENTED_EDGE('',*,*,#6958,.F.);
#9190=ORIENTED_EDGE('',*,*,#6959,.T.);
#9191=ORIENTED_EDGE('',*,*,#6950,.T.);
#9192=ORIENTED_EDGE('',*,*,#6959,.F.);
#9193=ORIENTED_EDGE('',*,*,#6933,.T.);
#9194=ORIENTED_EDGE('',*,*,#6954,.T.);
#9195=ORIENTED_EDGE('',*,*,#6937,.T.);
#9196=ORIENTED_EDGE('',*,*,#6952,.T.);
#9197=ORIENTED_EDGE('',*,*,#6941,.T.);
#9198=ORIENTED_EDGE('',*,*,#6951,.T.);
#9199=ORIENTED_EDGE('',*,*,#6945,.T.);
#9200=ORIENTED_EDGE('',*,*,#6953,.T.);
#9201=ORIENTED_EDGE('',*,*,#6957,.T.);
#9202=ORIENTED_EDGE('',*,*,#6960,.F.);
#9203=ORIENTED_EDGE('',*,*,#6961,.F.);
#9204=ORIENTED_EDGE('',*,*,#6962,.F.);
#9205=ORIENTED_EDGE('',*,*,#6963,.F.);
#9206=ORIENTED_EDGE('',*,*,#6964,.F.);
#9207=ORIENTED_EDGE('',*,*,#6965,.F.);
#9208=ORIENTED_EDGE('',*,*,#6966,.F.);
#9209=ORIENTED_EDGE('',*,*,#6967,.F.);
#9210=ORIENTED_EDGE('',*,*,#6968,.F.);
#9211=ORIENTED_EDGE('',*,*,#6969,.F.);
#9212=ORIENTED_EDGE('',*,*,#6970,.F.);
#9213=ORIENTED_EDGE('',*,*,#6971,.F.);
#9214=ORIENTED_EDGE('',*,*,#6972,.F.);
#9215=ORIENTED_EDGE('',*,*,#6973,.F.);
#9216=ORIENTED_EDGE('',*,*,#6974,.F.);
#9217=ORIENTED_EDGE('',*,*,#6975,.F.);
#9218=ORIENTED_EDGE('',*,*,#6961,.T.);
#9219=ORIENTED_EDGE('',*,*,#6976,.F.);
#9220=ORIENTED_EDGE('',*,*,#6973,.T.);
#9221=ORIENTED_EDGE('',*,*,#6977,.F.);
#9222=ORIENTED_EDGE('',*,*,#6969,.T.);
#9223=ORIENTED_EDGE('',*,*,#6978,.F.);
#9224=ORIENTED_EDGE('',*,*,#6965,.T.);
#9225=ORIENTED_EDGE('',*,*,#6979,.F.);
#9226=ORIENTED_EDGE('',*,*,#6980,.T.);
#9227=ORIENTED_EDGE('',*,*,#6970,.T.);
#9228=ORIENTED_EDGE('',*,*,#6977,.T.);
#9229=ORIENTED_EDGE('',*,*,#6972,.T.);
#9230=ORIENTED_EDGE('',*,*,#6981,.F.);
#9231=ORIENTED_EDGE('',*,*,#6966,.T.);
#9232=ORIENTED_EDGE('',*,*,#6978,.T.);
#9233=ORIENTED_EDGE('',*,*,#6968,.T.);
#9234=ORIENTED_EDGE('',*,*,#6982,.F.);
#9235=ORIENTED_EDGE('',*,*,#6960,.T.);
#9236=ORIENTED_EDGE('',*,*,#6983,.F.);
#9237=ORIENTED_EDGE('',*,*,#6974,.T.);
#9238=ORIENTED_EDGE('',*,*,#6976,.T.);
#9239=ORIENTED_EDGE('',*,*,#6962,.T.);
#9240=ORIENTED_EDGE('',*,*,#6979,.T.);
#9241=ORIENTED_EDGE('',*,*,#6964,.T.);
#9242=ORIENTED_EDGE('',*,*,#6984,.F.);
#9243=ORIENTED_EDGE('',*,*,#6980,.F.);
#9244=ORIENTED_EDGE('',*,*,#6985,.T.);
#9245=ORIENTED_EDGE('',*,*,#6986,.T.);
#9246=ORIENTED_EDGE('',*,*,#6985,.F.);
#9247=ORIENTED_EDGE('',*,*,#6986,.F.);
#9248=ORIENTED_EDGE('',*,*,#6987,.F.);
#9249=ORIENTED_EDGE('',*,*,#6988,.F.);
#9250=ORIENTED_EDGE('',*,*,#6989,.T.);
#9251=ORIENTED_EDGE('',*,*,#6987,.T.);
#9252=ORIENTED_EDGE('',*,*,#6989,.F.);
#9253=ORIENTED_EDGE('',*,*,#6963,.T.);
#9254=ORIENTED_EDGE('',*,*,#6984,.T.);
#9255=ORIENTED_EDGE('',*,*,#6967,.T.);
#9256=ORIENTED_EDGE('',*,*,#6982,.T.);
#9257=ORIENTED_EDGE('',*,*,#6971,.T.);
#9258=ORIENTED_EDGE('',*,*,#6981,.T.);
#9259=ORIENTED_EDGE('',*,*,#6975,.T.);
#9260=ORIENTED_EDGE('',*,*,#6983,.T.);
#9261=ORIENTED_EDGE('',*,*,#6988,.T.);
#9262=ORIENTED_EDGE('',*,*,#6990,.F.);
#9263=ORIENTED_EDGE('',*,*,#6991,.T.);
#9264=ORIENTED_EDGE('',*,*,#6992,.T.);
#9265=ORIENTED_EDGE('',*,*,#6991,.F.);
#9266=ORIENTED_EDGE('',*,*,#6992,.F.);
#9267=ORIENTED_EDGE('',*,*,#6993,.F.);
#9268=ORIENTED_EDGE('',*,*,#6994,.T.);
#9269=ORIENTED_EDGE('',*,*,#6995,.T.);
#9270=ORIENTED_EDGE('',*,*,#6994,.F.);
#9271=ORIENTED_EDGE('',*,*,#6995,.F.);
#9272=ORIENTED_EDGE('',*,*,#6996,.F.);
#9273=ORIENTED_EDGE('',*,*,#6997,.T.);
#9274=ORIENTED_EDGE('',*,*,#6998,.F.);
#9275=ORIENTED_EDGE('',*,*,#6997,.F.);
#9276=ORIENTED_EDGE('',*,*,#6999,.T.);
#9277=ORIENTED_EDGE('',*,*,#7000,.T.);
#9278=ORIENTED_EDGE('',*,*,#7001,.F.);
#9279=ORIENTED_EDGE('',*,*,#7002,.F.);
#9280=ORIENTED_EDGE('',*,*,#7003,.T.);
#9281=ORIENTED_EDGE('',*,*,#7002,.T.);
#9282=ORIENTED_EDGE('',*,*,#7004,.F.);
#9283=ORIENTED_EDGE('',*,*,#7005,.F.);
#9284=ORIENTED_EDGE('',*,*,#6998,.T.);
#9285=ORIENTED_EDGE('',*,*,#7006,.T.);
#9286=ORIENTED_EDGE('',*,*,#7005,.T.);
#9287=ORIENTED_EDGE('',*,*,#7007,.F.);
#9288=ORIENTED_EDGE('',*,*,#7008,.F.);
#9289=ORIENTED_EDGE('',*,*,#7009,.T.);
#9290=ORIENTED_EDGE('',*,*,#7008,.T.);
#9291=ORIENTED_EDGE('',*,*,#7010,.F.);
#9292=ORIENTED_EDGE('',*,*,#7000,.F.);
#9293=ORIENTED_EDGE('',*,*,#6996,.T.);
#9294=ORIENTED_EDGE('',*,*,#7010,.T.);
#9295=ORIENTED_EDGE('',*,*,#7007,.T.);
#9296=ORIENTED_EDGE('',*,*,#7004,.T.);
#9297=ORIENTED_EDGE('',*,*,#7001,.T.);
#9298=ORIENTED_EDGE('',*,*,#7009,.F.);
#9299=ORIENTED_EDGE('',*,*,#6999,.F.);
#9300=ORIENTED_EDGE('',*,*,#7003,.F.);
#9301=ORIENTED_EDGE('',*,*,#7006,.F.);
#9302=ORIENTED_EDGE('',*,*,#6990,.T.);
#9303=ORIENTED_EDGE('',*,*,#6993,.T.);
#9304=ORIENTED_EDGE('',*,*,#7011,.T.);
#9305=ORIENTED_EDGE('',*,*,#7011,.F.);
#9306=ORIENTED_EDGE('',*,*,#7012,.T.);
#9307=ORIENTED_EDGE('',*,*,#7013,.T.);
#9308=ORIENTED_EDGE('',*,*,#7012,.F.);
#9309=ORIENTED_EDGE('',*,*,#7013,.F.);
#9310=ORIENTED_EDGE('',*,*,#7014,.F.);
#9311=ORIENTED_EDGE('',*,*,#7015,.T.);
#9312=ORIENTED_EDGE('',*,*,#7016,.F.);
#9313=ORIENTED_EDGE('',*,*,#7017,.F.);
#9314=ORIENTED_EDGE('',*,*,#7018,.F.);
#9315=ORIENTED_EDGE('',*,*,#7019,.F.);
#9316=ORIENTED_EDGE('',*,*,#7015,.F.);
#9317=ORIENTED_EDGE('',*,*,#7020,.F.);
#9318=ORIENTED_EDGE('',*,*,#7021,.T.);
#9319=ORIENTED_EDGE('',*,*,#7022,.F.);
#9320=ORIENTED_EDGE('',*,*,#7021,.F.);
#9321=ORIENTED_EDGE('',*,*,#7023,.F.);
#9322=ORIENTED_EDGE('',*,*,#7017,.T.);
#9323=ORIENTED_EDGE('',*,*,#7024,.F.);
#9324=ORIENTED_EDGE('',*,*,#7025,.T.);
#9325=ORIENTED_EDGE('',*,*,#7020,.T.);
#9326=ORIENTED_EDGE('',*,*,#7014,.T.);
#9327=ORIENTED_EDGE('',*,*,#7019,.T.);
#9328=ORIENTED_EDGE('',*,*,#7026,.T.);
#9329=ORIENTED_EDGE('',*,*,#7027,.F.);
#9330=ORIENTED_EDGE('',*,*,#7026,.F.);
#9331=ORIENTED_EDGE('',*,*,#7018,.T.);
#9332=ORIENTED_EDGE('',*,*,#7023,.T.);
#9333=ORIENTED_EDGE('',*,*,#7016,.T.);
#9334=ORIENTED_EDGE('',*,*,#7025,.F.);
#9335=ORIENTED_EDGE('',*,*,#7028,.T.);
#9336=ORIENTED_EDGE('',*,*,#7029,.T.);
#9337=ORIENTED_EDGE('',*,*,#7030,.F.);
#9338=ORIENTED_EDGE('',*,*,#7031,.F.);
#9339=ORIENTED_EDGE('',*,*,#7032,.T.);
#9340=ORIENTED_EDGE('',*,*,#7031,.T.);
#9341=ORIENTED_EDGE('',*,*,#7033,.F.);
#9342=ORIENTED_EDGE('',*,*,#7034,.F.);
#9343=ORIENTED_EDGE('',*,*,#7027,.T.);
#9344=ORIENTED_EDGE('',*,*,#7035,.T.);
#9345=ORIENTED_EDGE('',*,*,#7034,.T.);
#9346=ORIENTED_EDGE('',*,*,#7036,.F.);
#9347=ORIENTED_EDGE('',*,*,#7037,.F.);
#9348=ORIENTED_EDGE('',*,*,#7038,.T.);
#9349=ORIENTED_EDGE('',*,*,#7037,.T.);
#9350=ORIENTED_EDGE('',*,*,#7039,.F.);
#9351=ORIENTED_EDGE('',*,*,#7029,.F.);
#9352=ORIENTED_EDGE('',*,*,#7024,.T.);
#9353=ORIENTED_EDGE('',*,*,#7039,.T.);
#9354=ORIENTED_EDGE('',*,*,#7036,.T.);
#9355=ORIENTED_EDGE('',*,*,#7033,.T.);
#9356=ORIENTED_EDGE('',*,*,#7030,.T.);
#9357=ORIENTED_EDGE('',*,*,#7022,.T.);
#9358=ORIENTED_EDGE('',*,*,#7038,.F.);
#9359=ORIENTED_EDGE('',*,*,#7028,.F.);
#9360=ORIENTED_EDGE('',*,*,#7032,.F.);
#9361=ORIENTED_EDGE('',*,*,#7035,.F.);
#9362=ORIENTED_EDGE('',*,*,#7040,.F.);
#9363=ORIENTED_EDGE('',*,*,#7041,.T.);
#9364=ORIENTED_EDGE('',*,*,#7042,.F.);
#9365=ORIENTED_EDGE('',*,*,#7043,.F.);
#9366=ORIENTED_EDGE('',*,*,#7044,.T.);
#9367=ORIENTED_EDGE('',*,*,#7045,.F.);
#9368=ORIENTED_EDGE('',*,*,#7044,.F.);
#9369=ORIENTED_EDGE('',*,*,#7046,.F.);
#9370=ORIENTED_EDGE('',*,*,#7047,.F.);
#9371=ORIENTED_EDGE('',*,*,#7041,.F.);
#9372=ORIENTED_EDGE('',*,*,#7048,.F.);
#9373=ORIENTED_EDGE('',*,*,#7049,.T.);
#9374=ORIENTED_EDGE('',*,*,#7050,.F.);
#9375=ORIENTED_EDGE('',*,*,#7051,.F.);
#9376=ORIENTED_EDGE('',*,*,#7052,.T.);
#9377=ORIENTED_EDGE('',*,*,#7053,.F.);
#9378=ORIENTED_EDGE('',*,*,#7052,.F.);
#9379=ORIENTED_EDGE('',*,*,#7054,.F.);
#9380=ORIENTED_EDGE('',*,*,#7055,.F.);
#9381=ORIENTED_EDGE('',*,*,#7049,.F.);
#9382=ORIENTED_EDGE('',*,*,#7056,.F.);
#9383=ORIENTED_EDGE('',*,*,#7057,.T.);
#9384=ORIENTED_EDGE('',*,*,#7058,.F.);
#9385=ORIENTED_EDGE('',*,*,#7059,.F.);
#9386=ORIENTED_EDGE('',*,*,#7060,.T.);
#9387=ORIENTED_EDGE('',*,*,#7061,.F.);
#9388=ORIENTED_EDGE('',*,*,#7060,.F.);
#9389=ORIENTED_EDGE('',*,*,#7062,.F.);
#9390=ORIENTED_EDGE('',*,*,#7063,.F.);
#9391=ORIENTED_EDGE('',*,*,#7057,.F.);
#9392=ORIENTED_EDGE('',*,*,#7064,.F.);
#9393=ORIENTED_EDGE('',*,*,#7065,.T.);
#9394=ORIENTED_EDGE('',*,*,#7066,.F.);
#9395=ORIENTED_EDGE('',*,*,#7067,.F.);
#9396=ORIENTED_EDGE('',*,*,#7068,.T.);
#9397=ORIENTED_EDGE('',*,*,#7069,.F.);
#9398=ORIENTED_EDGE('',*,*,#7068,.F.);
#9399=ORIENTED_EDGE('',*,*,#7070,.F.);
#9400=ORIENTED_EDGE('',*,*,#7071,.F.);
#9401=ORIENTED_EDGE('',*,*,#7065,.F.);
#9402=ORIENTED_EDGE('',*,*,#7042,.T.);
#9403=ORIENTED_EDGE('',*,*,#7040,.T.);
#9404=ORIENTED_EDGE('',*,*,#7047,.T.);
#9405=ORIENTED_EDGE('',*,*,#7072,.T.);
#9406=ORIENTED_EDGE('',*,*,#7058,.T.);
#9407=ORIENTED_EDGE('',*,*,#7056,.T.);
#9408=ORIENTED_EDGE('',*,*,#7063,.T.);
#9409=ORIENTED_EDGE('',*,*,#7073,.T.);
#9410=ORIENTED_EDGE('',*,*,#7074,.F.);
#9411=ORIENTED_EDGE('',*,*,#7075,.T.);
#9412=ORIENTED_EDGE('',*,*,#7076,.F.);
#9413=ORIENTED_EDGE('',*,*,#7077,.T.);
#9414=ORIENTED_EDGE('',*,*,#7050,.T.);
#9415=ORIENTED_EDGE('',*,*,#7048,.T.);
#9416=ORIENTED_EDGE('',*,*,#7055,.T.);
#9417=ORIENTED_EDGE('',*,*,#7078,.T.);
#9418=ORIENTED_EDGE('',*,*,#7066,.T.);
#9419=ORIENTED_EDGE('',*,*,#7064,.T.);
#9420=ORIENTED_EDGE('',*,*,#7071,.T.);
#9421=ORIENTED_EDGE('',*,*,#7079,.T.);
#9422=ORIENTED_EDGE('',*,*,#7080,.F.);
#9423=ORIENTED_EDGE('',*,*,#7081,.F.);
#9424=ORIENTED_EDGE('',*,*,#7082,.F.);
#9425=ORIENTED_EDGE('',*,*,#7083,.T.);
#9426=ORIENTED_EDGE('',*,*,#7074,.T.);
#9427=ORIENTED_EDGE('',*,*,#7084,.T.);
#9428=ORIENTED_EDGE('',*,*,#7085,.T.);
#9429=ORIENTED_EDGE('',*,*,#7086,.T.);
#9430=ORIENTED_EDGE('',*,*,#7087,.T.);
#9431=ORIENTED_EDGE('',*,*,#7088,.T.);
#9432=ORIENTED_EDGE('',*,*,#7082,.T.);
#9433=ORIENTED_EDGE('',*,*,#7089,.T.);
#9434=ORIENTED_EDGE('',*,*,#7090,.T.);
#9435=ORIENTED_EDGE('',*,*,#7091,.T.);
#9436=ORIENTED_EDGE('',*,*,#7092,.T.);
#9437=ORIENTED_EDGE('',*,*,#7093,.T.);
#9438=ORIENTED_EDGE('',*,*,#7046,.T.);
#9439=ORIENTED_EDGE('',*,*,#7043,.T.);
#9440=ORIENTED_EDGE('',*,*,#7077,.F.);
#9441=ORIENTED_EDGE('',*,*,#7094,.F.);
#9442=ORIENTED_EDGE('',*,*,#7095,.F.);
#9443=ORIENTED_EDGE('',*,*,#7084,.F.);
#9444=ORIENTED_EDGE('',*,*,#7073,.F.);
#9445=ORIENTED_EDGE('',*,*,#7062,.T.);
#9446=ORIENTED_EDGE('',*,*,#7059,.T.);
#9447=ORIENTED_EDGE('',*,*,#7072,.F.);
#9448=ORIENTED_EDGE('',*,*,#7095,.T.);
#9449=ORIENTED_EDGE('',*,*,#7096,.F.);
#9450=ORIENTED_EDGE('',*,*,#7097,.F.);
#9451=ORIENTED_EDGE('',*,*,#7085,.F.);
#9452=ORIENTED_EDGE('',*,*,#7097,.T.);
#9453=ORIENTED_EDGE('',*,*,#7098,.F.);
#9454=ORIENTED_EDGE('',*,*,#7099,.F.);
#9455=ORIENTED_EDGE('',*,*,#7086,.F.);
#9456=ORIENTED_EDGE('',*,*,#7045,.T.);
#9457=ORIENTED_EDGE('',*,*,#7053,.T.);
#9458=ORIENTED_EDGE('',*,*,#7061,.T.);
#9459=ORIENTED_EDGE('',*,*,#7069,.T.);
#9460=ORIENTED_EDGE('',*,*,#7099,.T.);
#9461=ORIENTED_EDGE('',*,*,#7100,.F.);
#9462=ORIENTED_EDGE('',*,*,#7101,.F.);
#9463=ORIENTED_EDGE('',*,*,#7087,.F.);
#9464=ORIENTED_EDGE('',*,*,#7054,.T.);
#9465=ORIENTED_EDGE('',*,*,#7051,.T.);
#9466=ORIENTED_EDGE('',*,*,#7083,.F.);
#9467=ORIENTED_EDGE('',*,*,#7088,.F.);
#9468=ORIENTED_EDGE('',*,*,#7101,.T.);
#9469=ORIENTED_EDGE('',*,*,#7102,.F.);
#9470=ORIENTED_EDGE('',*,*,#7079,.F.);
#9471=ORIENTED_EDGE('',*,*,#7070,.T.);
#9472=ORIENTED_EDGE('',*,*,#7067,.T.);
#9473=ORIENTED_EDGE('',*,*,#7078,.F.);
#9474=ORIENTED_EDGE('',*,*,#7081,.T.);
#9475=ORIENTED_EDGE('',*,*,#7103,.F.);
#9476=ORIENTED_EDGE('',*,*,#7104,.F.);
#9477=ORIENTED_EDGE('',*,*,#7089,.F.);
#9478=ORIENTED_EDGE('',*,*,#7104,.T.);
#9479=ORIENTED_EDGE('',*,*,#7105,.F.);
#9480=ORIENTED_EDGE('',*,*,#7106,.F.);
#9481=ORIENTED_EDGE('',*,*,#7090,.F.);
#9482=ORIENTED_EDGE('',*,*,#7106,.T.);
#9483=ORIENTED_EDGE('',*,*,#7107,.F.);
#9484=ORIENTED_EDGE('',*,*,#7108,.F.);
#9485=ORIENTED_EDGE('',*,*,#7091,.F.);
#9486=ORIENTED_EDGE('',*,*,#7108,.T.);
#9487=ORIENTED_EDGE('',*,*,#7109,.F.);
#9488=ORIENTED_EDGE('',*,*,#7110,.F.);
#9489=ORIENTED_EDGE('',*,*,#7092,.F.);
#9490=ORIENTED_EDGE('',*,*,#7110,.T.);
#9491=ORIENTED_EDGE('',*,*,#7111,.F.);
#9492=ORIENTED_EDGE('',*,*,#7075,.F.);
#9493=ORIENTED_EDGE('',*,*,#7093,.F.);
#9494=ORIENTED_EDGE('',*,*,#7076,.T.);
#9495=ORIENTED_EDGE('',*,*,#7111,.T.);
#9496=ORIENTED_EDGE('',*,*,#7109,.T.);
#9497=ORIENTED_EDGE('',*,*,#7107,.T.);
#9498=ORIENTED_EDGE('',*,*,#7105,.T.);
#9499=ORIENTED_EDGE('',*,*,#7103,.T.);
#9500=ORIENTED_EDGE('',*,*,#7080,.T.);
#9501=ORIENTED_EDGE('',*,*,#7102,.T.);
#9502=ORIENTED_EDGE('',*,*,#7100,.T.);
#9503=ORIENTED_EDGE('',*,*,#7098,.T.);
#9504=ORIENTED_EDGE('',*,*,#7096,.T.);
#9505=ORIENTED_EDGE('',*,*,#7094,.T.);
#9506=ORIENTED_EDGE('',*,*,#7112,.T.);
#9507=ORIENTED_EDGE('',*,*,#7113,.T.);
#9508=ORIENTED_EDGE('',*,*,#7114,.F.);
#9509=ORIENTED_EDGE('',*,*,#7115,.F.);
#9510=ORIENTED_EDGE('',*,*,#7116,.T.);
#9511=ORIENTED_EDGE('',*,*,#7115,.T.);
#9512=ORIENTED_EDGE('',*,*,#7117,.F.);
#9513=ORIENTED_EDGE('',*,*,#7118,.F.);
#9514=ORIENTED_EDGE('',*,*,#7119,.T.);
#9515=ORIENTED_EDGE('',*,*,#7118,.T.);
#9516=ORIENTED_EDGE('',*,*,#7120,.F.);
#9517=ORIENTED_EDGE('',*,*,#7121,.F.);
#9518=ORIENTED_EDGE('',*,*,#7122,.T.);
#9519=ORIENTED_EDGE('',*,*,#7121,.T.);
#9520=ORIENTED_EDGE('',*,*,#7123,.F.);
#9521=ORIENTED_EDGE('',*,*,#7124,.F.);
#9522=ORIENTED_EDGE('',*,*,#7125,.T.);
#9523=ORIENTED_EDGE('',*,*,#7124,.T.);
#9524=ORIENTED_EDGE('',*,*,#7126,.F.);
#9525=ORIENTED_EDGE('',*,*,#7127,.F.);
#9526=ORIENTED_EDGE('',*,*,#7128,.T.);
#9527=ORIENTED_EDGE('',*,*,#7127,.T.);
#9528=ORIENTED_EDGE('',*,*,#7129,.F.);
#9529=ORIENTED_EDGE('',*,*,#7130,.F.);
#9530=ORIENTED_EDGE('',*,*,#7131,.T.);
#9531=ORIENTED_EDGE('',*,*,#7130,.T.);
#9532=ORIENTED_EDGE('',*,*,#7132,.F.);
#9533=ORIENTED_EDGE('',*,*,#7133,.F.);
#9534=ORIENTED_EDGE('',*,*,#7134,.T.);
#9535=ORIENTED_EDGE('',*,*,#7133,.T.);
#9536=ORIENTED_EDGE('',*,*,#7135,.F.);
#9537=ORIENTED_EDGE('',*,*,#7113,.F.);
#9538=ORIENTED_EDGE('',*,*,#7135,.T.);
#9539=ORIENTED_EDGE('',*,*,#7132,.T.);
#9540=ORIENTED_EDGE('',*,*,#7129,.T.);
#9541=ORIENTED_EDGE('',*,*,#7126,.T.);
#9542=ORIENTED_EDGE('',*,*,#7123,.T.);
#9543=ORIENTED_EDGE('',*,*,#7120,.T.);
#9544=ORIENTED_EDGE('',*,*,#7117,.T.);
#9545=ORIENTED_EDGE('',*,*,#7114,.T.);
#9546=ORIENTED_EDGE('',*,*,#7134,.F.);
#9547=ORIENTED_EDGE('',*,*,#7112,.F.);
#9548=ORIENTED_EDGE('',*,*,#7116,.F.);
#9549=ORIENTED_EDGE('',*,*,#7119,.F.);
#9550=ORIENTED_EDGE('',*,*,#7122,.F.);
#9551=ORIENTED_EDGE('',*,*,#7125,.F.);
#9552=ORIENTED_EDGE('',*,*,#7128,.F.);
#9553=ORIENTED_EDGE('',*,*,#7131,.F.);
#9554=ORIENTED_EDGE('',*,*,#7136,.F.);
#9555=ORIENTED_EDGE('',*,*,#7137,.T.);
#9556=ORIENTED_EDGE('',*,*,#7138,.F.);
#9557=ORIENTED_EDGE('',*,*,#7139,.F.);
#9558=ORIENTED_EDGE('',*,*,#7140,.F.);
#9559=ORIENTED_EDGE('',*,*,#7139,.T.);
#9560=ORIENTED_EDGE('',*,*,#7141,.F.);
#9561=ORIENTED_EDGE('',*,*,#7142,.F.);
#9562=ORIENTED_EDGE('',*,*,#7143,.F.);
#9563=ORIENTED_EDGE('',*,*,#7142,.T.);
#9564=ORIENTED_EDGE('',*,*,#7144,.F.);
#9565=ORIENTED_EDGE('',*,*,#7145,.F.);
#9566=ORIENTED_EDGE('',*,*,#7146,.F.);
#9567=ORIENTED_EDGE('',*,*,#7145,.T.);
#9568=ORIENTED_EDGE('',*,*,#7147,.F.);
#9569=ORIENTED_EDGE('',*,*,#7148,.F.);
#9570=ORIENTED_EDGE('',*,*,#7149,.F.);
#9571=ORIENTED_EDGE('',*,*,#7148,.T.);
#9572=ORIENTED_EDGE('',*,*,#7150,.F.);
#9573=ORIENTED_EDGE('',*,*,#7151,.F.);
#9574=ORIENTED_EDGE('',*,*,#7152,.F.);
#9575=ORIENTED_EDGE('',*,*,#7151,.T.);
#9576=ORIENTED_EDGE('',*,*,#7153,.F.);
#9577=ORIENTED_EDGE('',*,*,#7154,.F.);
#9578=ORIENTED_EDGE('',*,*,#7155,.F.);
#9579=ORIENTED_EDGE('',*,*,#7154,.T.);
#9580=ORIENTED_EDGE('',*,*,#7156,.F.);
#9581=ORIENTED_EDGE('',*,*,#7157,.F.);
#9582=ORIENTED_EDGE('',*,*,#7158,.F.);
#9583=ORIENTED_EDGE('',*,*,#7157,.T.);
#9584=ORIENTED_EDGE('',*,*,#7159,.F.);
#9585=ORIENTED_EDGE('',*,*,#7137,.F.);
#9586=ORIENTED_EDGE('',*,*,#7158,.T.);
#9587=ORIENTED_EDGE('',*,*,#7136,.T.);
#9588=ORIENTED_EDGE('',*,*,#7140,.T.);
#9589=ORIENTED_EDGE('',*,*,#7143,.T.);
#9590=ORIENTED_EDGE('',*,*,#7146,.T.);
#9591=ORIENTED_EDGE('',*,*,#7149,.T.);
#9592=ORIENTED_EDGE('',*,*,#7152,.T.);
#9593=ORIENTED_EDGE('',*,*,#7155,.T.);
#9594=ORIENTED_EDGE('',*,*,#7159,.T.);
#9595=ORIENTED_EDGE('',*,*,#7156,.T.);
#9596=ORIENTED_EDGE('',*,*,#7153,.T.);
#9597=ORIENTED_EDGE('',*,*,#7150,.T.);
#9598=ORIENTED_EDGE('',*,*,#7147,.T.);
#9599=ORIENTED_EDGE('',*,*,#7144,.T.);
#9600=ORIENTED_EDGE('',*,*,#7141,.T.);
#9601=ORIENTED_EDGE('',*,*,#7138,.T.);
#9602=ORIENTED_EDGE('',*,*,#7160,.T.);
#9603=ORIENTED_EDGE('',*,*,#7161,.T.);
#9604=ORIENTED_EDGE('',*,*,#7162,.T.);
#9605=ORIENTED_EDGE('',*,*,#7163,.F.);
#9606=ORIENTED_EDGE('',*,*,#7164,.T.);
#9607=ORIENTED_EDGE('',*,*,#7165,.T.);
#9608=ORIENTED_EDGE('',*,*,#7166,.T.);
#9609=ORIENTED_EDGE('',*,*,#7161,.F.);
#9610=ORIENTED_EDGE('',*,*,#7167,.T.);
#9611=ORIENTED_EDGE('',*,*,#7168,.T.);
#9612=ORIENTED_EDGE('',*,*,#7169,.T.);
#9613=ORIENTED_EDGE('',*,*,#7165,.F.);
#9614=ORIENTED_EDGE('',*,*,#7170,.T.);
#9615=ORIENTED_EDGE('',*,*,#7171,.T.);
#9616=ORIENTED_EDGE('',*,*,#7172,.T.);
#9617=ORIENTED_EDGE('',*,*,#7168,.F.);
#9618=ORIENTED_EDGE('',*,*,#7173,.T.);
#9619=ORIENTED_EDGE('',*,*,#7174,.T.);
#9620=ORIENTED_EDGE('',*,*,#7175,.T.);
#9621=ORIENTED_EDGE('',*,*,#7171,.F.);
#9622=ORIENTED_EDGE('',*,*,#7176,.T.);
#9623=ORIENTED_EDGE('',*,*,#7163,.T.);
#9624=ORIENTED_EDGE('',*,*,#7177,.T.);
#9625=ORIENTED_EDGE('',*,*,#7174,.F.);
#9626=ORIENTED_EDGE('',*,*,#7176,.F.);
#9627=ORIENTED_EDGE('',*,*,#7173,.F.);
#9628=ORIENTED_EDGE('',*,*,#7170,.F.);
#9629=ORIENTED_EDGE('',*,*,#7167,.F.);
#9630=ORIENTED_EDGE('',*,*,#7164,.F.);
#9631=ORIENTED_EDGE('',*,*,#7160,.F.);
#9632=ORIENTED_EDGE('',*,*,#7177,.F.);
#9633=ORIENTED_EDGE('',*,*,#7162,.F.);
#9634=ORIENTED_EDGE('',*,*,#7166,.F.);
#9635=ORIENTED_EDGE('',*,*,#7169,.F.);
#9636=ORIENTED_EDGE('',*,*,#7172,.F.);
#9637=ORIENTED_EDGE('',*,*,#7175,.F.);
#9638=ORIENTED_EDGE('',*,*,#7178,.F.);
#9639=ORIENTED_EDGE('',*,*,#7179,.F.);
#9640=ORIENTED_EDGE('',*,*,#7180,.F.);
#9641=ORIENTED_EDGE('',*,*,#7181,.T.);
#9642=ORIENTED_EDGE('',*,*,#7179,.T.);
#9643=ORIENTED_EDGE('',*,*,#7181,.F.);
#9644=ORIENTED_EDGE('',*,*,#7182,.F.);
#9645=ORIENTED_EDGE('',*,*,#7183,.T.);
#9646=ORIENTED_EDGE('',*,*,#7180,.T.);
#9647=ORIENTED_EDGE('',*,*,#7183,.F.);
#9648=ORIENTED_EDGE('',*,*,#7184,.F.);
#9649=ORIENTED_EDGE('',*,*,#7185,.T.);
#9650=ORIENTED_EDGE('',*,*,#7182,.T.);
#9651=ORIENTED_EDGE('',*,*,#7185,.F.);
#9652=ORIENTED_EDGE('',*,*,#7184,.T.);
#9653=ORIENTED_EDGE('',*,*,#7186,.F.);
#9654=ORIENTED_EDGE('',*,*,#7187,.F.);
#9655=ORIENTED_EDGE('',*,*,#7188,.T.);
#9656=ORIENTED_EDGE('',*,*,#7186,.T.);
#9657=ORIENTED_EDGE('',*,*,#7188,.F.);
#9658=ORIENTED_EDGE('',*,*,#7178,.T.);
#9659=ORIENTED_EDGE('',*,*,#7189,.T.);
#9660=ORIENTED_EDGE('',*,*,#7187,.T.);
#9661=ORIENTED_EDGE('',*,*,#7189,.F.);
#9662=ORIENTED_EDGE('',*,*,#7190,.F.);
#9663=ORIENTED_EDGE('',*,*,#7191,.F.);
#9664=ORIENTED_EDGE('',*,*,#7192,.T.);
#9665=ORIENTED_EDGE('',*,*,#7193,.F.);
#9666=ORIENTED_EDGE('',*,*,#7194,.F.);
#9667=ORIENTED_EDGE('',*,*,#7192,.F.);
#9668=ORIENTED_EDGE('',*,*,#7193,.T.);
#9669=ORIENTED_EDGE('',*,*,#7194,.T.);
#9670=ORIENTED_EDGE('',*,*,#7195,.T.);
#9671=ORIENTED_EDGE('',*,*,#7196,.T.);
#9672=ORIENTED_EDGE('',*,*,#7195,.F.);
#9673=ORIENTED_EDGE('',*,*,#7197,.T.);
#9674=ORIENTED_EDGE('',*,*,#7198,.T.);
#9675=ORIENTED_EDGE('',*,*,#7199,.F.);
#9676=ORIENTED_EDGE('',*,*,#7198,.F.);
#9677=ORIENTED_EDGE('',*,*,#7199,.T.);
#9678=ORIENTED_EDGE('',*,*,#7200,.T.);
#9679=ORIENTED_EDGE('',*,*,#7201,.F.);
#9680=ORIENTED_EDGE('',*,*,#7200,.F.);
#9681=ORIENTED_EDGE('',*,*,#7196,.F.);
#9682=ORIENTED_EDGE('',*,*,#7201,.T.);
#9683=ORIENTED_EDGE('',*,*,#7202,.F.);
#9684=ORIENTED_EDGE('',*,*,#7203,.T.);
#9685=ORIENTED_EDGE('',*,*,#7190,.T.);
#9686=ORIENTED_EDGE('',*,*,#7191,.T.);
#9687=ORIENTED_EDGE('',*,*,#7203,.F.);
#9688=ORIENTED_EDGE('',*,*,#7202,.T.);
#9689=ORIENTED_EDGE('',*,*,#7204,.F.);
#9690=ORIENTED_EDGE('',*,*,#7204,.T.);
#9691=ORIENTED_EDGE('',*,*,#7205,.T.);
#9692=ORIENTED_EDGE('',*,*,#7197,.F.);
#9693=ORIENTED_EDGE('',*,*,#7205,.F.);
#9694=ORIENTED_EDGE('',*,*,#7206,.F.);
#9695=ORIENTED_EDGE('',*,*,#7207,.F.);
#9696=ORIENTED_EDGE('',*,*,#7208,.T.);
#9697=ORIENTED_EDGE('',*,*,#7209,.F.);
#9698=ORIENTED_EDGE('',*,*,#7210,.F.);
#9699=ORIENTED_EDGE('',*,*,#7208,.F.);
#9700=ORIENTED_EDGE('',*,*,#7211,.T.);
#9701=ORIENTED_EDGE('',*,*,#7212,.T.);
#9702=ORIENTED_EDGE('',*,*,#7209,.T.);
#9703=ORIENTED_EDGE('',*,*,#7210,.T.);
#9704=ORIENTED_EDGE('',*,*,#7212,.F.);
#9705=ORIENTED_EDGE('',*,*,#7213,.F.);
#9706=ORIENTED_EDGE('',*,*,#7214,.T.);
#9707=ORIENTED_EDGE('',*,*,#7215,.F.);
#9708=ORIENTED_EDGE('',*,*,#7216,.T.);
#9709=ORIENTED_EDGE('',*,*,#7213,.T.);
#9710=ORIENTED_EDGE('',*,*,#7216,.F.);
#9711=ORIENTED_EDGE('',*,*,#7217,.F.);
#9712=ORIENTED_EDGE('',*,*,#7218,.T.);
#9713=ORIENTED_EDGE('',*,*,#7215,.T.);
#9714=ORIENTED_EDGE('',*,*,#7218,.F.);
#9715=ORIENTED_EDGE('',*,*,#7219,.F.);
#9716=ORIENTED_EDGE('',*,*,#7220,.T.);
#9717=ORIENTED_EDGE('',*,*,#7217,.T.);
#9718=ORIENTED_EDGE('',*,*,#7220,.F.);
#9719=ORIENTED_EDGE('',*,*,#7219,.T.);
#9720=ORIENTED_EDGE('',*,*,#7211,.F.);
#9721=ORIENTED_EDGE('',*,*,#7206,.T.);
#9722=ORIENTED_EDGE('',*,*,#7207,.T.);
#9723=ORIENTED_EDGE('',*,*,#7221,.T.);
#9724=ORIENTED_EDGE('',*,*,#7214,.F.);
#9725=ORIENTED_EDGE('',*,*,#7221,.F.);
#9726=ORIENTED_EDGE('',*,*,#7222,.T.);
#9727=ORIENTED_EDGE('',*,*,#7222,.F.);
#9728=ORIENTED_EDGE('',*,*,#7223,.T.);
#9729=ORIENTED_EDGE('',*,*,#7223,.F.);
#9730=ORIENTED_EDGE('',*,*,#7224,.T.);
#9731=ORIENTED_EDGE('',*,*,#7224,.F.);
#9732=ORIENTED_EDGE('',*,*,#7225,.T.);
#9733=ORIENTED_EDGE('',*,*,#7225,.F.);
#9734=ORIENTED_EDGE('',*,*,#7226,.T.);
#9735=ORIENTED_EDGE('',*,*,#7226,.F.);
#9736=ORIENTED_EDGE('',*,*,#7227,.T.);
#9737=ORIENTED_EDGE('',*,*,#7227,.F.);
#9738=ORIENTED_EDGE('',*,*,#7228,.T.);
#9739=ORIENTED_EDGE('',*,*,#7228,.F.);
#9740=ORIENTED_EDGE('',*,*,#7229,.F.);
#9741=ORIENTED_EDGE('',*,*,#7230,.F.);
#9742=ORIENTED_EDGE('',*,*,#7231,.F.);
#9743=ORIENTED_EDGE('',*,*,#7232,.F.);
#9744=ORIENTED_EDGE('',*,*,#7231,.T.);
#9745=ORIENTED_EDGE('',*,*,#7233,.F.);
#9746=ORIENTED_EDGE('',*,*,#7234,.T.);
#9747=ORIENTED_EDGE('',*,*,#7235,.F.);
#9748=ORIENTED_EDGE('',*,*,#7236,.T.);
#9749=ORIENTED_EDGE('',*,*,#7237,.F.);
#9750=ORIENTED_EDGE('',*,*,#7238,.T.);
#9751=ORIENTED_EDGE('',*,*,#7239,.F.);
#9752=ORIENTED_EDGE('',*,*,#7238,.F.);
#9753=ORIENTED_EDGE('',*,*,#7240,.F.);
#9754=ORIENTED_EDGE('',*,*,#7241,.T.);
#9755=ORIENTED_EDGE('',*,*,#7242,.F.);
#9756=ORIENTED_EDGE('',*,*,#7243,.T.);
#9757=ORIENTED_EDGE('',*,*,#7244,.F.);
#9758=ORIENTED_EDGE('',*,*,#7245,.T.);
#9759=ORIENTED_EDGE('',*,*,#7246,.F.);
#9760=ORIENTED_EDGE('',*,*,#7247,.T.);
#9761=ORIENTED_EDGE('',*,*,#7248,.F.);
#9762=ORIENTED_EDGE('',*,*,#7230,.T.);
#9763=ORIENTED_EDGE('',*,*,#7249,.T.);
#9764=ORIENTED_EDGE('',*,*,#7250,.T.);
#9765=ORIENTED_EDGE('',*,*,#7233,.T.);
#9766=ORIENTED_EDGE('',*,*,#7251,.F.);
#9767=ORIENTED_EDGE('',*,*,#7252,.F.);
#9768=ORIENTED_EDGE('',*,*,#7234,.F.);
#9769=ORIENTED_EDGE('',*,*,#7250,.F.);
#9770=ORIENTED_EDGE('',*,*,#7252,.T.);
#9771=ORIENTED_EDGE('',*,*,#7253,.T.);
#9772=ORIENTED_EDGE('',*,*,#7254,.T.);
#9773=ORIENTED_EDGE('',*,*,#7235,.T.);
#9774=ORIENTED_EDGE('',*,*,#7255,.F.);
#9775=ORIENTED_EDGE('',*,*,#7256,.F.);
#9776=ORIENTED_EDGE('',*,*,#7236,.F.);
#9777=ORIENTED_EDGE('',*,*,#7254,.F.);
#9778=ORIENTED_EDGE('',*,*,#7256,.T.);
#9779=ORIENTED_EDGE('',*,*,#7257,.T.);
#9780=ORIENTED_EDGE('',*,*,#7258,.T.);
#9781=ORIENTED_EDGE('',*,*,#7259,.T.);
#9782=ORIENTED_EDGE('',*,*,#7240,.T.);
#9783=ORIENTED_EDGE('',*,*,#7237,.T.);
#9784=ORIENTED_EDGE('',*,*,#7260,.F.);
#9785=ORIENTED_EDGE('',*,*,#7261,.F.);
#9786=ORIENTED_EDGE('',*,*,#7241,.F.);
#9787=ORIENTED_EDGE('',*,*,#7259,.F.);
#9788=ORIENTED_EDGE('',*,*,#7261,.T.);
#9789=ORIENTED_EDGE('',*,*,#7262,.T.);
#9790=ORIENTED_EDGE('',*,*,#7263,.T.);
#9791=ORIENTED_EDGE('',*,*,#7242,.T.);
#9792=ORIENTED_EDGE('',*,*,#7264,.F.);
#9793=ORIENTED_EDGE('',*,*,#7265,.F.);
#9794=ORIENTED_EDGE('',*,*,#7243,.F.);
#9795=ORIENTED_EDGE('',*,*,#7263,.F.);
#9796=ORIENTED_EDGE('',*,*,#7265,.T.);
#9797=ORIENTED_EDGE('',*,*,#7266,.T.);
#9798=ORIENTED_EDGE('',*,*,#7267,.T.);
#9799=ORIENTED_EDGE('',*,*,#7244,.T.);
#9800=ORIENTED_EDGE('',*,*,#7245,.F.);
#9801=ORIENTED_EDGE('',*,*,#7267,.F.);
#9802=ORIENTED_EDGE('',*,*,#7268,.F.);
#9803=ORIENTED_EDGE('',*,*,#7269,.F.);
#9804=ORIENTED_EDGE('',*,*,#7270,.F.);
#9805=ORIENTED_EDGE('',*,*,#7271,.T.);
#9806=ORIENTED_EDGE('',*,*,#7257,.F.);
#9807=ORIENTED_EDGE('',*,*,#7255,.T.);
#9808=ORIENTED_EDGE('',*,*,#7253,.F.);
#9809=ORIENTED_EDGE('',*,*,#7251,.T.);
#9810=ORIENTED_EDGE('',*,*,#7249,.F.);
#9811=ORIENTED_EDGE('',*,*,#7229,.T.);
#9812=ORIENTED_EDGE('',*,*,#7272,.F.);
#9813=ORIENTED_EDGE('',*,*,#7273,.T.);
#9814=ORIENTED_EDGE('',*,*,#7274,.F.);
#9815=ORIENTED_EDGE('',*,*,#7268,.T.);
#9816=ORIENTED_EDGE('',*,*,#7266,.F.);
#9817=ORIENTED_EDGE('',*,*,#7264,.T.);
#9818=ORIENTED_EDGE('',*,*,#7262,.F.);
#9819=ORIENTED_EDGE('',*,*,#7260,.T.);
#9820=ORIENTED_EDGE('',*,*,#7258,.F.);
#9821=ORIENTED_EDGE('',*,*,#7271,.F.);
#9822=ORIENTED_EDGE('',*,*,#7232,.T.);
#9823=ORIENTED_EDGE('',*,*,#7248,.T.);
#9824=ORIENTED_EDGE('',*,*,#7275,.T.);
#9825=ORIENTED_EDGE('',*,*,#7272,.T.);
#9826=ORIENTED_EDGE('',*,*,#7247,.F.);
#9827=ORIENTED_EDGE('',*,*,#7276,.F.);
#9828=ORIENTED_EDGE('',*,*,#7273,.F.);
#9829=ORIENTED_EDGE('',*,*,#7275,.F.);
#9830=ORIENTED_EDGE('',*,*,#7239,.T.);
#9831=ORIENTED_EDGE('',*,*,#7270,.T.);
#9832=ORIENTED_EDGE('',*,*,#7269,.T.);
#9833=ORIENTED_EDGE('',*,*,#7274,.T.);
#9834=ORIENTED_EDGE('',*,*,#7276,.T.);
#9835=ORIENTED_EDGE('',*,*,#7246,.T.);
#9836=ORIENTED_EDGE('',*,*,#7277,.F.);
#9837=ORIENTED_EDGE('',*,*,#7278,.T.);
#9838=ORIENTED_EDGE('',*,*,#7279,.F.);
#9839=ORIENTED_EDGE('',*,*,#7280,.T.);
#9840=ORIENTED_EDGE('',*,*,#7277,.T.);
#9841=ORIENTED_EDGE('',*,*,#7280,.F.);
#9842=ORIENTED_EDGE('',*,*,#7279,.T.);
#9843=ORIENTED_EDGE('',*,*,#7281,.F.);
#9844=ORIENTED_EDGE('',*,*,#7281,.T.);
#9845=ORIENTED_EDGE('',*,*,#7282,.T.);
#9846=ORIENTED_EDGE('',*,*,#7278,.F.);
#9847=ORIENTED_EDGE('',*,*,#7282,.F.);
#9848=ORIENTED_EDGE('',*,*,#7283,.F.);
#9849=ORIENTED_EDGE('',*,*,#7284,.T.);
#9850=ORIENTED_EDGE('',*,*,#7285,.F.);
#9851=ORIENTED_EDGE('',*,*,#7286,.T.);
#9852=ORIENTED_EDGE('',*,*,#7283,.T.);
#9853=ORIENTED_EDGE('',*,*,#7286,.F.);
#9854=ORIENTED_EDGE('',*,*,#7285,.T.);
#9855=ORIENTED_EDGE('',*,*,#7287,.F.);
#9856=ORIENTED_EDGE('',*,*,#7287,.T.);
#9857=ORIENTED_EDGE('',*,*,#7288,.T.);
#9858=ORIENTED_EDGE('',*,*,#7284,.F.);
#9859=ORIENTED_EDGE('',*,*,#7288,.F.);
#9860=ORIENTED_EDGE('',*,*,#7289,.T.);
#9861=ORIENTED_EDGE('',*,*,#7290,.T.);
#9862=ORIENTED_EDGE('',*,*,#7291,.T.);
#9863=ORIENTED_EDGE('',*,*,#7292,.F.);
#9864=ORIENTED_EDGE('',*,*,#7293,.T.);
#9865=ORIENTED_EDGE('',*,*,#7294,.T.);
#9866=ORIENTED_EDGE('',*,*,#7295,.T.);
#9867=ORIENTED_EDGE('',*,*,#7290,.F.);
#9868=ORIENTED_EDGE('',*,*,#7296,.T.);
#9869=ORIENTED_EDGE('',*,*,#7297,.T.);
#9870=ORIENTED_EDGE('',*,*,#7298,.T.);
#9871=ORIENTED_EDGE('',*,*,#7294,.F.);
#9872=ORIENTED_EDGE('',*,*,#7299,.T.);
#9873=ORIENTED_EDGE('',*,*,#7300,.T.);
#9874=ORIENTED_EDGE('',*,*,#7301,.T.);
#9875=ORIENTED_EDGE('',*,*,#7297,.F.);
#9876=ORIENTED_EDGE('',*,*,#7302,.T.);
#9877=ORIENTED_EDGE('',*,*,#7303,.T.);
#9878=ORIENTED_EDGE('',*,*,#7304,.T.);
#9879=ORIENTED_EDGE('',*,*,#7300,.F.);
#9880=ORIENTED_EDGE('',*,*,#7305,.T.);
#9881=ORIENTED_EDGE('',*,*,#7292,.T.);
#9882=ORIENTED_EDGE('',*,*,#7306,.T.);
#9883=ORIENTED_EDGE('',*,*,#7303,.F.);
#9884=ORIENTED_EDGE('',*,*,#7305,.F.);
#9885=ORIENTED_EDGE('',*,*,#7302,.F.);
#9886=ORIENTED_EDGE('',*,*,#7299,.F.);
#9887=ORIENTED_EDGE('',*,*,#7296,.F.);
#9888=ORIENTED_EDGE('',*,*,#7293,.F.);
#9889=ORIENTED_EDGE('',*,*,#7289,.F.);
#9890=ORIENTED_EDGE('',*,*,#7306,.F.);
#9891=ORIENTED_EDGE('',*,*,#7291,.F.);
#9892=ORIENTED_EDGE('',*,*,#7295,.F.);
#9893=ORIENTED_EDGE('',*,*,#7298,.F.);
#9894=ORIENTED_EDGE('',*,*,#7301,.F.);
#9895=ORIENTED_EDGE('',*,*,#7304,.F.);
#9896=ORIENTED_EDGE('',*,*,#7307,.F.);
#9897=ORIENTED_EDGE('',*,*,#7308,.F.);
#9898=ORIENTED_EDGE('',*,*,#7309,.F.);
#9899=ORIENTED_EDGE('',*,*,#7310,.T.);
#9900=ORIENTED_EDGE('',*,*,#7308,.T.);
#9901=ORIENTED_EDGE('',*,*,#7310,.F.);
#9902=ORIENTED_EDGE('',*,*,#7311,.F.);
#9903=ORIENTED_EDGE('',*,*,#7312,.T.);
#9904=ORIENTED_EDGE('',*,*,#7309,.T.);
#9905=ORIENTED_EDGE('',*,*,#7312,.F.);
#9906=ORIENTED_EDGE('',*,*,#7313,.F.);
#9907=ORIENTED_EDGE('',*,*,#7314,.T.);
#9908=ORIENTED_EDGE('',*,*,#7311,.T.);
#9909=ORIENTED_EDGE('',*,*,#7314,.F.);
#9910=ORIENTED_EDGE('',*,*,#7313,.T.);
#9911=ORIENTED_EDGE('',*,*,#7315,.F.);
#9912=ORIENTED_EDGE('',*,*,#7316,.F.);
#9913=ORIENTED_EDGE('',*,*,#7317,.T.);
#9914=ORIENTED_EDGE('',*,*,#7315,.T.);
#9915=ORIENTED_EDGE('',*,*,#7317,.F.);
#9916=ORIENTED_EDGE('',*,*,#7307,.T.);
#9917=ORIENTED_EDGE('',*,*,#7318,.T.);
#9918=ORIENTED_EDGE('',*,*,#7316,.T.);
#9919=ORIENTED_EDGE('',*,*,#7318,.F.);
#9920=ORIENTED_EDGE('',*,*,#7319,.F.);
#9921=ORIENTED_EDGE('',*,*,#7320,.T.);
#9922=ORIENTED_EDGE('',*,*,#7321,.T.);
#9923=ORIENTED_EDGE('',*,*,#7320,.F.);
#9924=ORIENTED_EDGE('',*,*,#7321,.F.);
#9925=ORIENTED_EDGE('',*,*,#7322,.T.);
#9926=ORIENTED_EDGE('',*,*,#7323,.F.);
#9927=ORIENTED_EDGE('',*,*,#7324,.F.);
#9928=ORIENTED_EDGE('',*,*,#7325,.F.);
#9929=ORIENTED_EDGE('',*,*,#7322,.F.);
#9930=ORIENTED_EDGE('',*,*,#7326,.T.);
#9931=ORIENTED_EDGE('',*,*,#7324,.T.);
#9932=ORIENTED_EDGE('',*,*,#7326,.F.);
#9933=ORIENTED_EDGE('',*,*,#7325,.T.);
#9934=ORIENTED_EDGE('',*,*,#7327,.T.);
#9935=ORIENTED_EDGE('',*,*,#7328,.T.);
#9936=ORIENTED_EDGE('',*,*,#7327,.F.);
#9937=ORIENTED_EDGE('',*,*,#7329,.F.);
#9938=ORIENTED_EDGE('',*,*,#7330,.T.);
#9939=ORIENTED_EDGE('',*,*,#7331,.T.);
#9940=ORIENTED_EDGE('',*,*,#7330,.F.);
#9941=ORIENTED_EDGE('',*,*,#7331,.F.);
#9942=ORIENTED_EDGE('',*,*,#7319,.T.);
#9943=ORIENTED_EDGE('',*,*,#7332,.F.);
#9944=ORIENTED_EDGE('',*,*,#7333,.T.);
#9945=ORIENTED_EDGE('',*,*,#7323,.T.);
#9946=ORIENTED_EDGE('',*,*,#7333,.F.);
#9947=ORIENTED_EDGE('',*,*,#7332,.T.);
#9948=ORIENTED_EDGE('',*,*,#7328,.F.);
#9949=ORIENTED_EDGE('',*,*,#7329,.T.);
#9950=ORIENTED_EDGE('',*,*,#7334,.F.);
#9951=ORIENTED_EDGE('',*,*,#7335,.T.);
#9952=ORIENTED_EDGE('',*,*,#7336,.F.);
#9953=ORIENTED_EDGE('',*,*,#7335,.F.);
#9954=ORIENTED_EDGE('',*,*,#7334,.T.);
#9955=ORIENTED_EDGE('',*,*,#7337,.F.);
#9956=ORIENTED_EDGE('',*,*,#7337,.T.);
#9957=ORIENTED_EDGE('',*,*,#7338,.T.);
#9958=ORIENTED_EDGE('',*,*,#7339,.T.);
#9959=ORIENTED_EDGE('',*,*,#7338,.F.);
#9960=ORIENTED_EDGE('',*,*,#7340,.F.);
#9961=ORIENTED_EDGE('',*,*,#7341,.T.);
#9962=ORIENTED_EDGE('',*,*,#7342,.T.);
#9963=ORIENTED_EDGE('',*,*,#7341,.F.);
#9964=ORIENTED_EDGE('',*,*,#7340,.T.);
#9965=ORIENTED_EDGE('',*,*,#7336,.T.);
#9966=ORIENTED_EDGE('',*,*,#7342,.F.);
#9967=ORIENTED_EDGE('',*,*,#7339,.F.);
#9968=ORIENTED_EDGE('',*,*,#7343,.F.);
#9969=ORIENTED_EDGE('',*,*,#7344,.T.);
#9970=ORIENTED_EDGE('',*,*,#7345,.T.);
#9971=ORIENTED_EDGE('',*,*,#7344,.F.);
#9972=ORIENTED_EDGE('',*,*,#7346,.F.);
#9973=ORIENTED_EDGE('',*,*,#7347,.T.);
#9974=ORIENTED_EDGE('',*,*,#7348,.T.);
#9975=ORIENTED_EDGE('',*,*,#7347,.F.);
#9976=ORIENTED_EDGE('',*,*,#7346,.T.);
#9977=ORIENTED_EDGE('',*,*,#7343,.T.);
#9978=ORIENTED_EDGE('',*,*,#7348,.F.);
#9979=ORIENTED_EDGE('',*,*,#7345,.F.);
#9980=ORIENTED_EDGE('',*,*,#7349,.F.);
#9981=ORIENTED_EDGE('',*,*,#7350,.T.);
#9982=ORIENTED_EDGE('',*,*,#7351,.T.);
#9983=ORIENTED_EDGE('',*,*,#7350,.F.);
#9984=ORIENTED_EDGE('',*,*,#7349,.T.);
#9985=ORIENTED_EDGE('',*,*,#7351,.F.);
#9986=ORIENTED_EDGE('',*,*,#7352,.F.);
#9987=ORIENTED_EDGE('',*,*,#7353,.T.);
#9988=ORIENTED_EDGE('',*,*,#7354,.T.);
#9989=ORIENTED_EDGE('',*,*,#7353,.F.);
#9990=ORIENTED_EDGE('',*,*,#7352,.T.);
#9991=ORIENTED_EDGE('',*,*,#7354,.F.);
#9992=ORIENTED_EDGE('',*,*,#7355,.F.);
#9993=ORIENTED_EDGE('',*,*,#7356,.T.);
#9994=ORIENTED_EDGE('',*,*,#7357,.T.);
#9995=ORIENTED_EDGE('',*,*,#7356,.F.);
#9996=ORIENTED_EDGE('',*,*,#7358,.F.);
#9997=ORIENTED_EDGE('',*,*,#7359,.T.);
#9998=ORIENTED_EDGE('',*,*,#7360,.T.);
#9999=ORIENTED_EDGE('',*,*,#7359,.F.);
#10000=ORIENTED_EDGE('',*,*,#7358,.T.);
#10001=ORIENTED_EDGE('',*,*,#7355,.T.);
#10002=ORIENTED_EDGE('',*,*,#7360,.F.);
#10003=ORIENTED_EDGE('',*,*,#7357,.F.);
#10004=ORIENTED_EDGE('',*,*,#7361,.F.);
#10005=ORIENTED_EDGE('',*,*,#7362,.F.);
#10006=ORIENTED_EDGE('',*,*,#7363,.F.);
#10007=ORIENTED_EDGE('',*,*,#7364,.T.);
#10008=ORIENTED_EDGE('',*,*,#7365,.F.);
#10009=ORIENTED_EDGE('',*,*,#7366,.F.);
#10010=ORIENTED_EDGE('',*,*,#7367,.F.);
#10011=ORIENTED_EDGE('',*,*,#7368,.F.);
#10012=ORIENTED_EDGE('',*,*,#7364,.F.);
#10013=ORIENTED_EDGE('',*,*,#7369,.F.);
#10014=ORIENTED_EDGE('',*,*,#7370,.F.);
#10015=ORIENTED_EDGE('',*,*,#7371,.T.);
#10016=ORIENTED_EDGE('',*,*,#7372,.F.);
#10017=ORIENTED_EDGE('',*,*,#7373,.F.);
#10018=ORIENTED_EDGE('',*,*,#7374,.F.);
#10019=ORIENTED_EDGE('',*,*,#7371,.F.);
#10020=ORIENTED_EDGE('',*,*,#7375,.F.);
#10021=ORIENTED_EDGE('',*,*,#7376,.T.);
#10022=ORIENTED_EDGE('',*,*,#7362,.T.);
#10023=ORIENTED_EDGE('',*,*,#7377,.T.);
#10024=ORIENTED_EDGE('',*,*,#7378,.F.);
#10025=ORIENTED_EDGE('',*,*,#7377,.F.);
#10026=ORIENTED_EDGE('',*,*,#7361,.T.);
#10027=ORIENTED_EDGE('',*,*,#7363,.T.);
#10028=ORIENTED_EDGE('',*,*,#7376,.F.);
#10029=ORIENTED_EDGE('',*,*,#7373,.T.);
#10030=ORIENTED_EDGE('',*,*,#7372,.T.);
#10031=ORIENTED_EDGE('',*,*,#7374,.T.);
#10032=ORIENTED_EDGE('',*,*,#7379,.T.);
#10033=ORIENTED_EDGE('',*,*,#7380,.T.);
#10034=ORIENTED_EDGE('',*,*,#7381,.T.);
#10035=ORIENTED_EDGE('',*,*,#7382,.T.);
#10036=ORIENTED_EDGE('',*,*,#7383,.T.);
#10037=ORIENTED_EDGE('',*,*,#7384,.T.);
#10038=ORIENTED_EDGE('',*,*,#7380,.F.);
#10039=ORIENTED_EDGE('',*,*,#7379,.F.);
#10040=ORIENTED_EDGE('',*,*,#7381,.F.);
#10041=ORIENTED_EDGE('',*,*,#7385,.T.);
#10042=ORIENTED_EDGE('',*,*,#7386,.F.);
#10043=ORIENTED_EDGE('',*,*,#7387,.F.);
#10044=ORIENTED_EDGE('',*,*,#7385,.F.);
#10045=ORIENTED_EDGE('',*,*,#7388,.F.);
#10046=ORIENTED_EDGE('',*,*,#7389,.F.);
#10047=ORIENTED_EDGE('',*,*,#7390,.T.);
#10048=ORIENTED_EDGE('',*,*,#7383,.F.);
#10049=ORIENTED_EDGE('',*,*,#7382,.F.);
#10050=ORIENTED_EDGE('',*,*,#7384,.F.);
#10051=ORIENTED_EDGE('',*,*,#7390,.F.);
#10052=ORIENTED_EDGE('',*,*,#7391,.F.);
#10053=ORIENTED_EDGE('',*,*,#7392,.T.);
#10054=ORIENTED_EDGE('',*,*,#7365,.T.);
#10055=ORIENTED_EDGE('',*,*,#7368,.T.);
#10056=ORIENTED_EDGE('',*,*,#7393,.T.);
#10057=ORIENTED_EDGE('',*,*,#7394,.F.);
#10058=ORIENTED_EDGE('',*,*,#7393,.F.);
#10059=ORIENTED_EDGE('',*,*,#7367,.T.);
#10060=ORIENTED_EDGE('',*,*,#7366,.T.);
#10061=ORIENTED_EDGE('',*,*,#7392,.F.);
#10062=ORIENTED_EDGE('',*,*,#7369,.T.);
#10063=ORIENTED_EDGE('',*,*,#7370,.T.);
#10064=ORIENTED_EDGE('',*,*,#7388,.T.);
#10065=ORIENTED_EDGE('',*,*,#7389,.T.);
#10066=ORIENTED_EDGE('',*,*,#7386,.T.);
#10067=ORIENTED_EDGE('',*,*,#7387,.T.);
#10068=ORIENTED_EDGE('',*,*,#7375,.T.);
#10069=ORIENTED_EDGE('',*,*,#7391,.T.);
#10070=ORIENTED_EDGE('',*,*,#7395,.T.);
#10071=ORIENTED_EDGE('',*,*,#7396,.T.);
#10072=ORIENTED_EDGE('',*,*,#7397,.F.);
#10073=ORIENTED_EDGE('',*,*,#7398,.T.);
#10074=ORIENTED_EDGE('',*,*,#7399,.F.);
#10075=ORIENTED_EDGE('',*,*,#7400,.T.);
#10076=ORIENTED_EDGE('',*,*,#7401,.F.);
#10077=ORIENTED_EDGE('',*,*,#7402,.T.);
#10078=ORIENTED_EDGE('',*,*,#7403,.F.);
#10079=ORIENTED_EDGE('',*,*,#7404,.T.);
#10080=ORIENTED_EDGE('',*,*,#7405,.F.);
#10081=ORIENTED_EDGE('',*,*,#7406,.T.);
#10082=ORIENTED_EDGE('',*,*,#7407,.F.);
#10083=ORIENTED_EDGE('',*,*,#7408,.T.);
#10084=ORIENTED_EDGE('',*,*,#7409,.F.);
#10085=ORIENTED_EDGE('',*,*,#7410,.T.);
#10086=ORIENTED_EDGE('',*,*,#7411,.F.);
#10087=ORIENTED_EDGE('',*,*,#7412,.T.);
#10088=ORIENTED_EDGE('',*,*,#7413,.F.);
#10089=ORIENTED_EDGE('',*,*,#7414,.T.);
#10090=ORIENTED_EDGE('',*,*,#7415,.F.);
#10091=ORIENTED_EDGE('',*,*,#7416,.T.);
#10092=ORIENTED_EDGE('',*,*,#7417,.F.);
#10093=ORIENTED_EDGE('',*,*,#7418,.T.);
#10094=ORIENTED_EDGE('',*,*,#7419,.F.);
#10095=ORIENTED_EDGE('',*,*,#7420,.T.);
#10096=ORIENTED_EDGE('',*,*,#7421,.F.);
#10097=ORIENTED_EDGE('',*,*,#7422,.T.);
#10098=ORIENTED_EDGE('',*,*,#7423,.F.);
#10099=ORIENTED_EDGE('',*,*,#7424,.T.);
#10100=ORIENTED_EDGE('',*,*,#7425,.F.);
#10101=ORIENTED_EDGE('',*,*,#7426,.T.);
#10102=ORIENTED_EDGE('',*,*,#7427,.F.);
#10103=ORIENTED_EDGE('',*,*,#7428,.T.);
#10104=ORIENTED_EDGE('',*,*,#7429,.F.);
#10105=ORIENTED_EDGE('',*,*,#7430,.T.);
#10106=ORIENTED_EDGE('',*,*,#7431,.F.);
#10107=ORIENTED_EDGE('',*,*,#7432,.T.);
#10108=ORIENTED_EDGE('',*,*,#7433,.F.);
#10109=ORIENTED_EDGE('',*,*,#7434,.T.);
#10110=ORIENTED_EDGE('',*,*,#7435,.F.);
#10111=ORIENTED_EDGE('',*,*,#7436,.F.);
#10112=ORIENTED_EDGE('',*,*,#7437,.T.);
#10113=ORIENTED_EDGE('',*,*,#7395,.F.);
#10114=ORIENTED_EDGE('',*,*,#7437,.F.);
#10115=ORIENTED_EDGE('',*,*,#7436,.T.);
#10116=ORIENTED_EDGE('',*,*,#7378,.T.);
#10117=ORIENTED_EDGE('',*,*,#7438,.F.);
#10118=ORIENTED_EDGE('',*,*,#7439,.T.);
#10119=ORIENTED_EDGE('',*,*,#7440,.T.);
#10120=ORIENTED_EDGE('',*,*,#7441,.T.);
#10121=ORIENTED_EDGE('',*,*,#7442,.T.);
#10122=ORIENTED_EDGE('',*,*,#7443,.T.);
#10123=ORIENTED_EDGE('',*,*,#7444,.T.);
#10124=ORIENTED_EDGE('',*,*,#7445,.T.);
#10125=ORIENTED_EDGE('',*,*,#7446,.T.);
#10126=ORIENTED_EDGE('',*,*,#7447,.T.);
#10127=ORIENTED_EDGE('',*,*,#7448,.T.);
#10128=ORIENTED_EDGE('',*,*,#7449,.T.);
#10129=ORIENTED_EDGE('',*,*,#7450,.T.);
#10130=ORIENTED_EDGE('',*,*,#7451,.T.);
#10131=ORIENTED_EDGE('',*,*,#7452,.T.);
#10132=ORIENTED_EDGE('',*,*,#7453,.T.);
#10133=ORIENTED_EDGE('',*,*,#7454,.T.);
#10134=ORIENTED_EDGE('',*,*,#7455,.T.);
#10135=ORIENTED_EDGE('',*,*,#7456,.T.);
#10136=ORIENTED_EDGE('',*,*,#7457,.T.);
#10137=ORIENTED_EDGE('',*,*,#7458,.T.);
#10138=ORIENTED_EDGE('',*,*,#7459,.T.);
#10139=ORIENTED_EDGE('',*,*,#7460,.T.);
#10140=ORIENTED_EDGE('',*,*,#7461,.T.);
#10141=ORIENTED_EDGE('',*,*,#7462,.T.);
#10142=ORIENTED_EDGE('',*,*,#7463,.T.);
#10143=ORIENTED_EDGE('',*,*,#7464,.T.);
#10144=ORIENTED_EDGE('',*,*,#7465,.T.);
#10145=ORIENTED_EDGE('',*,*,#7466,.T.);
#10146=ORIENTED_EDGE('',*,*,#7467,.T.);
#10147=ORIENTED_EDGE('',*,*,#7468,.T.);
#10148=ORIENTED_EDGE('',*,*,#7469,.T.);
#10149=ORIENTED_EDGE('',*,*,#7470,.T.);
#10150=ORIENTED_EDGE('',*,*,#7471,.T.);
#10151=ORIENTED_EDGE('',*,*,#7472,.T.);
#10152=ORIENTED_EDGE('',*,*,#7473,.T.);
#10153=ORIENTED_EDGE('',*,*,#7474,.T.);
#10154=ORIENTED_EDGE('',*,*,#7475,.T.);
#10155=ORIENTED_EDGE('',*,*,#7476,.T.);
#10156=ORIENTED_EDGE('',*,*,#7477,.T.);
#10157=ORIENTED_EDGE('',*,*,#7478,.T.);
#10158=ORIENTED_EDGE('',*,*,#7479,.F.);
#10159=ORIENTED_EDGE('',*,*,#7480,.T.);
#10160=ORIENTED_EDGE('',*,*,#7438,.T.);
#10161=ORIENTED_EDGE('',*,*,#7480,.F.);
#10162=ORIENTED_EDGE('',*,*,#7479,.T.);
#10163=ORIENTED_EDGE('',*,*,#7394,.T.);
#10164=ORIENTED_EDGE('',*,*,#7481,.F.);
#10165=ORIENTED_EDGE('',*,*,#7439,.F.);
#10166=ORIENTED_EDGE('',*,*,#7482,.F.);
#10167=ORIENTED_EDGE('',*,*,#7396,.F.);
#10168=ORIENTED_EDGE('',*,*,#7482,.T.);
#10169=ORIENTED_EDGE('',*,*,#7478,.F.);
#10170=ORIENTED_EDGE('',*,*,#7483,.T.);
#10171=ORIENTED_EDGE('',*,*,#7397,.T.);
#10172=ORIENTED_EDGE('',*,*,#7483,.F.);
#10173=ORIENTED_EDGE('',*,*,#7477,.F.);
#10174=ORIENTED_EDGE('',*,*,#7484,.F.);
#10175=ORIENTED_EDGE('',*,*,#7398,.F.);
#10176=ORIENTED_EDGE('',*,*,#7484,.T.);
#10177=ORIENTED_EDGE('',*,*,#7476,.F.);
#10178=ORIENTED_EDGE('',*,*,#7485,.T.);
#10179=ORIENTED_EDGE('',*,*,#7399,.T.);
#10180=ORIENTED_EDGE('',*,*,#7485,.F.);
#10181=ORIENTED_EDGE('',*,*,#7475,.F.);
#10182=ORIENTED_EDGE('',*,*,#7486,.F.);
#10183=ORIENTED_EDGE('',*,*,#7400,.F.);
#10184=ORIENTED_EDGE('',*,*,#7486,.T.);
#10185=ORIENTED_EDGE('',*,*,#7474,.F.);
#10186=ORIENTED_EDGE('',*,*,#7487,.T.);
#10187=ORIENTED_EDGE('',*,*,#7401,.T.);
#10188=ORIENTED_EDGE('',*,*,#7487,.F.);
#10189=ORIENTED_EDGE('',*,*,#7473,.F.);
#10190=ORIENTED_EDGE('',*,*,#7488,.F.);
#10191=ORIENTED_EDGE('',*,*,#7402,.F.);
#10192=ORIENTED_EDGE('',*,*,#7488,.T.);
#10193=ORIENTED_EDGE('',*,*,#7472,.F.);
#10194=ORIENTED_EDGE('',*,*,#7489,.T.);
#10195=ORIENTED_EDGE('',*,*,#7403,.T.);
#10196=ORIENTED_EDGE('',*,*,#7489,.F.);
#10197=ORIENTED_EDGE('',*,*,#7471,.F.);
#10198=ORIENTED_EDGE('',*,*,#7490,.F.);
#10199=ORIENTED_EDGE('',*,*,#7404,.F.);
#10200=ORIENTED_EDGE('',*,*,#7490,.T.);
#10201=ORIENTED_EDGE('',*,*,#7470,.F.);
#10202=ORIENTED_EDGE('',*,*,#7491,.T.);
#10203=ORIENTED_EDGE('',*,*,#7405,.T.);
#10204=ORIENTED_EDGE('',*,*,#7491,.F.);
#10205=ORIENTED_EDGE('',*,*,#7469,.F.);
#10206=ORIENTED_EDGE('',*,*,#7492,.F.);
#10207=ORIENTED_EDGE('',*,*,#7406,.F.);
#10208=ORIENTED_EDGE('',*,*,#7492,.T.);
#10209=ORIENTED_EDGE('',*,*,#7468,.F.);
#10210=ORIENTED_EDGE('',*,*,#7493,.T.);
#10211=ORIENTED_EDGE('',*,*,#7407,.T.);
#10212=ORIENTED_EDGE('',*,*,#7493,.F.);
#10213=ORIENTED_EDGE('',*,*,#7467,.F.);
#10214=ORIENTED_EDGE('',*,*,#7494,.F.);
#10215=ORIENTED_EDGE('',*,*,#7408,.F.);
#10216=ORIENTED_EDGE('',*,*,#7494,.T.);
#10217=ORIENTED_EDGE('',*,*,#7466,.F.);
#10218=ORIENTED_EDGE('',*,*,#7495,.T.);
#10219=ORIENTED_EDGE('',*,*,#7409,.T.);
#10220=ORIENTED_EDGE('',*,*,#7495,.F.);
#10221=ORIENTED_EDGE('',*,*,#7465,.F.);
#10222=ORIENTED_EDGE('',*,*,#7496,.F.);
#10223=ORIENTED_EDGE('',*,*,#7410,.F.);
#10224=ORIENTED_EDGE('',*,*,#7496,.T.);
#10225=ORIENTED_EDGE('',*,*,#7464,.F.);
#10226=ORIENTED_EDGE('',*,*,#7497,.T.);
#10227=ORIENTED_EDGE('',*,*,#7411,.T.);
#10228=ORIENTED_EDGE('',*,*,#7497,.F.);
#10229=ORIENTED_EDGE('',*,*,#7463,.F.);
#10230=ORIENTED_EDGE('',*,*,#7498,.F.);
#10231=ORIENTED_EDGE('',*,*,#7412,.F.);
#10232=ORIENTED_EDGE('',*,*,#7498,.T.);
#10233=ORIENTED_EDGE('',*,*,#7462,.F.);
#10234=ORIENTED_EDGE('',*,*,#7499,.T.);
#10235=ORIENTED_EDGE('',*,*,#7413,.T.);
#10236=ORIENTED_EDGE('',*,*,#7499,.F.);
#10237=ORIENTED_EDGE('',*,*,#7461,.F.);
#10238=ORIENTED_EDGE('',*,*,#7500,.F.);
#10239=ORIENTED_EDGE('',*,*,#7414,.F.);
#10240=ORIENTED_EDGE('',*,*,#7500,.T.);
#10241=ORIENTED_EDGE('',*,*,#7460,.F.);
#10242=ORIENTED_EDGE('',*,*,#7501,.T.);
#10243=ORIENTED_EDGE('',*,*,#7415,.T.);
#10244=ORIENTED_EDGE('',*,*,#7501,.F.);
#10245=ORIENTED_EDGE('',*,*,#7459,.F.);
#10246=ORIENTED_EDGE('',*,*,#7502,.F.);
#10247=ORIENTED_EDGE('',*,*,#7416,.F.);
#10248=ORIENTED_EDGE('',*,*,#7502,.T.);
#10249=ORIENTED_EDGE('',*,*,#7458,.F.);
#10250=ORIENTED_EDGE('',*,*,#7503,.T.);
#10251=ORIENTED_EDGE('',*,*,#7417,.T.);
#10252=ORIENTED_EDGE('',*,*,#7503,.F.);
#10253=ORIENTED_EDGE('',*,*,#7457,.F.);
#10254=ORIENTED_EDGE('',*,*,#7504,.F.);
#10255=ORIENTED_EDGE('',*,*,#7418,.F.);
#10256=ORIENTED_EDGE('',*,*,#7504,.T.);
#10257=ORIENTED_EDGE('',*,*,#7456,.F.);
#10258=ORIENTED_EDGE('',*,*,#7505,.T.);
#10259=ORIENTED_EDGE('',*,*,#7419,.T.);
#10260=ORIENTED_EDGE('',*,*,#7505,.F.);
#10261=ORIENTED_EDGE('',*,*,#7455,.F.);
#10262=ORIENTED_EDGE('',*,*,#7506,.F.);
#10263=ORIENTED_EDGE('',*,*,#7420,.F.);
#10264=ORIENTED_EDGE('',*,*,#7506,.T.);
#10265=ORIENTED_EDGE('',*,*,#7454,.F.);
#10266=ORIENTED_EDGE('',*,*,#7507,.T.);
#10267=ORIENTED_EDGE('',*,*,#7421,.T.);
#10268=ORIENTED_EDGE('',*,*,#7507,.F.);
#10269=ORIENTED_EDGE('',*,*,#7453,.F.);
#10270=ORIENTED_EDGE('',*,*,#7508,.F.);
#10271=ORIENTED_EDGE('',*,*,#7422,.F.);
#10272=ORIENTED_EDGE('',*,*,#7508,.T.);
#10273=ORIENTED_EDGE('',*,*,#7452,.F.);
#10274=ORIENTED_EDGE('',*,*,#7509,.T.);
#10275=ORIENTED_EDGE('',*,*,#7423,.T.);
#10276=ORIENTED_EDGE('',*,*,#7509,.F.);
#10277=ORIENTED_EDGE('',*,*,#7451,.F.);
#10278=ORIENTED_EDGE('',*,*,#7510,.F.);
#10279=ORIENTED_EDGE('',*,*,#7424,.F.);
#10280=ORIENTED_EDGE('',*,*,#7510,.T.);
#10281=ORIENTED_EDGE('',*,*,#7450,.F.);
#10282=ORIENTED_EDGE('',*,*,#7511,.T.);
#10283=ORIENTED_EDGE('',*,*,#7425,.T.);
#10284=ORIENTED_EDGE('',*,*,#7511,.F.);
#10285=ORIENTED_EDGE('',*,*,#7449,.F.);
#10286=ORIENTED_EDGE('',*,*,#7512,.F.);
#10287=ORIENTED_EDGE('',*,*,#7426,.F.);
#10288=ORIENTED_EDGE('',*,*,#7512,.T.);
#10289=ORIENTED_EDGE('',*,*,#7448,.F.);
#10290=ORIENTED_EDGE('',*,*,#7513,.T.);
#10291=ORIENTED_EDGE('',*,*,#7427,.T.);
#10292=ORIENTED_EDGE('',*,*,#7513,.F.);
#10293=ORIENTED_EDGE('',*,*,#7447,.F.);
#10294=ORIENTED_EDGE('',*,*,#7514,.F.);
#10295=ORIENTED_EDGE('',*,*,#7428,.F.);
#10296=ORIENTED_EDGE('',*,*,#7514,.T.);
#10297=ORIENTED_EDGE('',*,*,#7446,.F.);
#10298=ORIENTED_EDGE('',*,*,#7515,.T.);
#10299=ORIENTED_EDGE('',*,*,#7429,.T.);
#10300=ORIENTED_EDGE('',*,*,#7515,.F.);
#10301=ORIENTED_EDGE('',*,*,#7445,.F.);
#10302=ORIENTED_EDGE('',*,*,#7516,.F.);
#10303=ORIENTED_EDGE('',*,*,#7430,.F.);
#10304=ORIENTED_EDGE('',*,*,#7516,.T.);
#10305=ORIENTED_EDGE('',*,*,#7444,.F.);
#10306=ORIENTED_EDGE('',*,*,#7517,.T.);
#10307=ORIENTED_EDGE('',*,*,#7431,.T.);
#10308=ORIENTED_EDGE('',*,*,#7518,.F.);
#10309=ORIENTED_EDGE('',*,*,#7432,.F.);
#10310=ORIENTED_EDGE('',*,*,#7517,.F.);
#10311=ORIENTED_EDGE('',*,*,#7443,.F.);
#10312=ORIENTED_EDGE('',*,*,#7481,.T.);
#10313=ORIENTED_EDGE('',*,*,#7435,.T.);
#10314=ORIENTED_EDGE('',*,*,#7519,.T.);
#10315=ORIENTED_EDGE('',*,*,#7440,.F.);
#10316=ORIENTED_EDGE('',*,*,#7520,.F.);
#10317=ORIENTED_EDGE('',*,*,#7441,.F.);
#10318=ORIENTED_EDGE('',*,*,#7519,.F.);
#10319=ORIENTED_EDGE('',*,*,#7434,.F.);
#10320=ORIENTED_EDGE('',*,*,#7518,.T.);
#10321=ORIENTED_EDGE('',*,*,#7442,.F.);
#10322=ORIENTED_EDGE('',*,*,#7520,.T.);
#10323=ORIENTED_EDGE('',*,*,#7433,.T.);
#10324=ORIENTED_EDGE('',*,*,#7521,.F.);
#10325=ORIENTED_EDGE('',*,*,#7522,.T.);
#10326=ORIENTED_EDGE('',*,*,#7523,.T.);
#10327=ORIENTED_EDGE('',*,*,#7522,.F.);
#10328=ORIENTED_EDGE('',*,*,#7523,.F.);
#10329=ORIENTED_EDGE('',*,*,#7524,.T.);
#10330=ORIENTED_EDGE('',*,*,#7525,.F.);
#10331=ORIENTED_EDGE('',*,*,#7526,.F.);
#10332=ORIENTED_EDGE('',*,*,#7527,.F.);
#10333=ORIENTED_EDGE('',*,*,#7524,.F.);
#10334=ORIENTED_EDGE('',*,*,#7528,.T.);
#10335=ORIENTED_EDGE('',*,*,#7526,.T.);
#10336=ORIENTED_EDGE('',*,*,#7528,.F.);
#10337=ORIENTED_EDGE('',*,*,#7527,.T.);
#10338=ORIENTED_EDGE('',*,*,#7529,.T.);
#10339=ORIENTED_EDGE('',*,*,#7530,.T.);
#10340=ORIENTED_EDGE('',*,*,#7529,.F.);
#10341=ORIENTED_EDGE('',*,*,#7530,.F.);
#10342=ORIENTED_EDGE('',*,*,#7521,.T.);
#10343=ORIENTED_EDGE('',*,*,#7531,.F.);
#10344=ORIENTED_EDGE('',*,*,#7532,.T.);
#10345=ORIENTED_EDGE('',*,*,#7525,.T.);
#10346=ORIENTED_EDGE('',*,*,#7532,.F.);
#10347=ORIENTED_EDGE('',*,*,#7531,.T.);
#10348=ORIENTED_EDGE('',*,*,#7533,.F.);
#10349=ORIENTED_EDGE('',*,*,#7534,.T.);
#10350=ORIENTED_EDGE('',*,*,#7535,.T.);
#10351=ORIENTED_EDGE('',*,*,#7534,.F.);
#10352=ORIENTED_EDGE('',*,*,#7536,.F.);
#10353=ORIENTED_EDGE('',*,*,#7537,.T.);
#10354=ORIENTED_EDGE('',*,*,#7538,.T.);
#10355=ORIENTED_EDGE('',*,*,#7537,.F.);
#10356=ORIENTED_EDGE('',*,*,#7536,.T.);
#10357=ORIENTED_EDGE('',*,*,#7533,.T.);
#10358=ORIENTED_EDGE('',*,*,#7538,.F.);
#10359=ORIENTED_EDGE('',*,*,#7535,.F.);
#10360=ORIENTED_EDGE('',*,*,#7539,.F.);
#10361=ORIENTED_EDGE('',*,*,#7540,.T.);
#10362=ORIENTED_EDGE('',*,*,#7541,.T.);
#10363=ORIENTED_EDGE('',*,*,#7540,.F.);
#10364=ORIENTED_EDGE('',*,*,#7542,.F.);
#10365=ORIENTED_EDGE('',*,*,#7543,.T.);
#10366=ORIENTED_EDGE('',*,*,#7544,.T.);
#10367=ORIENTED_EDGE('',*,*,#7543,.F.);
#10368=ORIENTED_EDGE('',*,*,#7542,.T.);
#10369=ORIENTED_EDGE('',*,*,#7539,.T.);
#10370=ORIENTED_EDGE('',*,*,#7544,.F.);
#10371=ORIENTED_EDGE('',*,*,#7541,.F.);
#10372=ORIENTED_EDGE('',*,*,#7545,.F.);
#10373=ORIENTED_EDGE('',*,*,#7546,.T.);
#10374=ORIENTED_EDGE('',*,*,#7547,.T.);
#10375=ORIENTED_EDGE('',*,*,#7546,.F.);
#10376=ORIENTED_EDGE('',*,*,#7545,.T.);
#10377=ORIENTED_EDGE('',*,*,#7547,.F.);
#10378=ORIENTED_EDGE('',*,*,#7548,.F.);
#10379=ORIENTED_EDGE('',*,*,#7549,.T.);
#10380=ORIENTED_EDGE('',*,*,#7550,.T.);
#10381=ORIENTED_EDGE('',*,*,#7549,.F.);
#10382=ORIENTED_EDGE('',*,*,#7548,.T.);
#10383=ORIENTED_EDGE('',*,*,#7550,.F.);
#10384=ORIENTED_EDGE('',*,*,#7551,.F.);
#10385=ORIENTED_EDGE('',*,*,#7552,.T.);
#10386=ORIENTED_EDGE('',*,*,#7553,.T.);
#10387=ORIENTED_EDGE('',*,*,#7552,.F.);
#10388=ORIENTED_EDGE('',*,*,#7554,.F.);
#10389=ORIENTED_EDGE('',*,*,#7555,.T.);
#10390=ORIENTED_EDGE('',*,*,#7556,.T.);
#10391=ORIENTED_EDGE('',*,*,#7555,.F.);
#10392=ORIENTED_EDGE('',*,*,#7554,.T.);
#10393=ORIENTED_EDGE('',*,*,#7551,.T.);
#10394=ORIENTED_EDGE('',*,*,#7556,.F.);
#10395=ORIENTED_EDGE('',*,*,#7553,.F.);
#10396=ORIENTED_EDGE('',*,*,#7557,.F.);
#10397=ORIENTED_EDGE('',*,*,#7558,.F.);
#10398=ORIENTED_EDGE('',*,*,#7559,.F.);
#10399=ORIENTED_EDGE('',*,*,#7560,.T.);
#10400=ORIENTED_EDGE('',*,*,#7561,.F.);
#10401=ORIENTED_EDGE('',*,*,#7562,.F.);
#10402=ORIENTED_EDGE('',*,*,#7563,.F.);
#10403=ORIENTED_EDGE('',*,*,#7564,.F.);
#10404=ORIENTED_EDGE('',*,*,#7560,.F.);
#10405=ORIENTED_EDGE('',*,*,#7565,.F.);
#10406=ORIENTED_EDGE('',*,*,#7566,.F.);
#10407=ORIENTED_EDGE('',*,*,#7567,.T.);
#10408=ORIENTED_EDGE('',*,*,#7568,.F.);
#10409=ORIENTED_EDGE('',*,*,#7569,.F.);
#10410=ORIENTED_EDGE('',*,*,#7570,.F.);
#10411=ORIENTED_EDGE('',*,*,#7567,.F.);
#10412=ORIENTED_EDGE('',*,*,#7571,.F.);
#10413=ORIENTED_EDGE('',*,*,#7572,.T.);
#10414=ORIENTED_EDGE('',*,*,#7558,.T.);
#10415=ORIENTED_EDGE('',*,*,#7573,.T.);
#10416=ORIENTED_EDGE('',*,*,#7574,.F.);
#10417=ORIENTED_EDGE('',*,*,#7573,.F.);
#10418=ORIENTED_EDGE('',*,*,#7557,.T.);
#10419=ORIENTED_EDGE('',*,*,#7559,.T.);
#10420=ORIENTED_EDGE('',*,*,#7572,.F.);
#10421=ORIENTED_EDGE('',*,*,#7569,.T.);
#10422=ORIENTED_EDGE('',*,*,#7568,.T.);
#10423=ORIENTED_EDGE('',*,*,#7570,.T.);
#10424=ORIENTED_EDGE('',*,*,#7575,.T.);
#10425=ORIENTED_EDGE('',*,*,#7576,.T.);
#10426=ORIENTED_EDGE('',*,*,#7577,.T.);
#10427=ORIENTED_EDGE('',*,*,#7578,.T.);
#10428=ORIENTED_EDGE('',*,*,#7579,.T.);
#10429=ORIENTED_EDGE('',*,*,#7580,.T.);
#10430=ORIENTED_EDGE('',*,*,#7576,.F.);
#10431=ORIENTED_EDGE('',*,*,#7575,.F.);
#10432=ORIENTED_EDGE('',*,*,#7577,.F.);
#10433=ORIENTED_EDGE('',*,*,#7581,.T.);
#10434=ORIENTED_EDGE('',*,*,#7582,.F.);
#10435=ORIENTED_EDGE('',*,*,#7583,.F.);
#10436=ORIENTED_EDGE('',*,*,#7581,.F.);
#10437=ORIENTED_EDGE('',*,*,#7584,.F.);
#10438=ORIENTED_EDGE('',*,*,#7585,.F.);
#10439=ORIENTED_EDGE('',*,*,#7586,.T.);
#10440=ORIENTED_EDGE('',*,*,#7579,.F.);
#10441=ORIENTED_EDGE('',*,*,#7578,.F.);
#10442=ORIENTED_EDGE('',*,*,#7580,.F.);
#10443=ORIENTED_EDGE('',*,*,#7586,.F.);
#10444=ORIENTED_EDGE('',*,*,#7587,.F.);
#10445=ORIENTED_EDGE('',*,*,#7588,.T.);
#10446=ORIENTED_EDGE('',*,*,#7561,.T.);
#10447=ORIENTED_EDGE('',*,*,#7564,.T.);
#10448=ORIENTED_EDGE('',*,*,#7589,.T.);
#10449=ORIENTED_EDGE('',*,*,#7590,.F.);
#10450=ORIENTED_EDGE('',*,*,#7589,.F.);
#10451=ORIENTED_EDGE('',*,*,#7563,.T.);
#10452=ORIENTED_EDGE('',*,*,#7562,.T.);
#10453=ORIENTED_EDGE('',*,*,#7588,.F.);
#10454=ORIENTED_EDGE('',*,*,#7565,.T.);
#10455=ORIENTED_EDGE('',*,*,#7566,.T.);
#10456=ORIENTED_EDGE('',*,*,#7584,.T.);
#10457=ORIENTED_EDGE('',*,*,#7585,.T.);
#10458=ORIENTED_EDGE('',*,*,#7582,.T.);
#10459=ORIENTED_EDGE('',*,*,#7583,.T.);
#10460=ORIENTED_EDGE('',*,*,#7571,.T.);
#10461=ORIENTED_EDGE('',*,*,#7587,.T.);
#10462=ORIENTED_EDGE('',*,*,#7591,.T.);
#10463=ORIENTED_EDGE('',*,*,#7592,.T.);
#10464=ORIENTED_EDGE('',*,*,#7593,.F.);
#10465=ORIENTED_EDGE('',*,*,#7594,.T.);
#10466=ORIENTED_EDGE('',*,*,#7595,.F.);
#10467=ORIENTED_EDGE('',*,*,#7596,.T.);
#10468=ORIENTED_EDGE('',*,*,#7597,.F.);
#10469=ORIENTED_EDGE('',*,*,#7598,.T.);
#10470=ORIENTED_EDGE('',*,*,#7599,.F.);
#10471=ORIENTED_EDGE('',*,*,#7600,.T.);
#10472=ORIENTED_EDGE('',*,*,#7601,.F.);
#10473=ORIENTED_EDGE('',*,*,#7602,.T.);
#10474=ORIENTED_EDGE('',*,*,#7603,.F.);
#10475=ORIENTED_EDGE('',*,*,#7604,.T.);
#10476=ORIENTED_EDGE('',*,*,#7605,.F.);
#10477=ORIENTED_EDGE('',*,*,#7606,.T.);
#10478=ORIENTED_EDGE('',*,*,#7607,.F.);
#10479=ORIENTED_EDGE('',*,*,#7608,.T.);
#10480=ORIENTED_EDGE('',*,*,#7609,.F.);
#10481=ORIENTED_EDGE('',*,*,#7610,.T.);
#10482=ORIENTED_EDGE('',*,*,#7611,.F.);
#10483=ORIENTED_EDGE('',*,*,#7612,.T.);
#10484=ORIENTED_EDGE('',*,*,#7613,.F.);
#10485=ORIENTED_EDGE('',*,*,#7614,.T.);
#10486=ORIENTED_EDGE('',*,*,#7615,.F.);
#10487=ORIENTED_EDGE('',*,*,#7616,.T.);
#10488=ORIENTED_EDGE('',*,*,#7617,.F.);
#10489=ORIENTED_EDGE('',*,*,#7618,.T.);
#10490=ORIENTED_EDGE('',*,*,#7619,.F.);
#10491=ORIENTED_EDGE('',*,*,#7620,.T.);
#10492=ORIENTED_EDGE('',*,*,#7621,.F.);
#10493=ORIENTED_EDGE('',*,*,#7622,.T.);
#10494=ORIENTED_EDGE('',*,*,#7623,.F.);
#10495=ORIENTED_EDGE('',*,*,#7624,.T.);
#10496=ORIENTED_EDGE('',*,*,#7625,.F.);
#10497=ORIENTED_EDGE('',*,*,#7626,.T.);
#10498=ORIENTED_EDGE('',*,*,#7627,.F.);
#10499=ORIENTED_EDGE('',*,*,#7628,.T.);
#10500=ORIENTED_EDGE('',*,*,#7629,.F.);
#10501=ORIENTED_EDGE('',*,*,#7630,.T.);
#10502=ORIENTED_EDGE('',*,*,#7631,.F.);
#10503=ORIENTED_EDGE('',*,*,#7632,.T.);
#10504=ORIENTED_EDGE('',*,*,#7633,.F.);
#10505=ORIENTED_EDGE('',*,*,#7634,.T.);
#10506=ORIENTED_EDGE('',*,*,#7635,.F.);
#10507=ORIENTED_EDGE('',*,*,#7636,.T.);
#10508=ORIENTED_EDGE('',*,*,#7637,.F.);
#10509=ORIENTED_EDGE('',*,*,#7638,.T.);
#10510=ORIENTED_EDGE('',*,*,#7639,.F.);
#10511=ORIENTED_EDGE('',*,*,#7640,.T.);
#10512=ORIENTED_EDGE('',*,*,#7641,.F.);
#10513=ORIENTED_EDGE('',*,*,#7642,.T.);
#10514=ORIENTED_EDGE('',*,*,#7643,.F.);
#10515=ORIENTED_EDGE('',*,*,#7644,.T.);
#10516=ORIENTED_EDGE('',*,*,#7645,.F.);
#10517=ORIENTED_EDGE('',*,*,#7646,.T.);
#10518=ORIENTED_EDGE('',*,*,#7647,.F.);
#10519=ORIENTED_EDGE('',*,*,#7648,.T.);
#10520=ORIENTED_EDGE('',*,*,#7649,.F.);
#10521=ORIENTED_EDGE('',*,*,#7650,.T.);
#10522=ORIENTED_EDGE('',*,*,#7651,.F.);
#10523=ORIENTED_EDGE('',*,*,#7652,.T.);
#10524=ORIENTED_EDGE('',*,*,#7653,.F.);
#10525=ORIENTED_EDGE('',*,*,#7654,.T.);
#10526=ORIENTED_EDGE('',*,*,#7655,.F.);
#10527=ORIENTED_EDGE('',*,*,#7656,.T.);
#10528=ORIENTED_EDGE('',*,*,#7657,.F.);
#10529=ORIENTED_EDGE('',*,*,#7658,.T.);
#10530=ORIENTED_EDGE('',*,*,#7659,.F.);
#10531=ORIENTED_EDGE('',*,*,#7660,.T.);
#10532=ORIENTED_EDGE('',*,*,#7661,.F.);
#10533=ORIENTED_EDGE('',*,*,#7662,.T.);
#10534=ORIENTED_EDGE('',*,*,#7663,.F.);
#10535=ORIENTED_EDGE('',*,*,#7664,.T.);
#10536=ORIENTED_EDGE('',*,*,#7665,.F.);
#10537=ORIENTED_EDGE('',*,*,#7666,.T.);
#10538=ORIENTED_EDGE('',*,*,#7667,.F.);
#10539=ORIENTED_EDGE('',*,*,#7668,.T.);
#10540=ORIENTED_EDGE('',*,*,#7669,.F.);
#10541=ORIENTED_EDGE('',*,*,#7670,.T.);
#10542=ORIENTED_EDGE('',*,*,#7671,.F.);
#10543=ORIENTED_EDGE('',*,*,#7672,.F.);
#10544=ORIENTED_EDGE('',*,*,#7673,.T.);
#10545=ORIENTED_EDGE('',*,*,#7591,.F.);
#10546=ORIENTED_EDGE('',*,*,#7673,.F.);
#10547=ORIENTED_EDGE('',*,*,#7672,.T.);
#10548=ORIENTED_EDGE('',*,*,#7574,.T.);
#10549=ORIENTED_EDGE('',*,*,#7674,.F.);
#10550=ORIENTED_EDGE('',*,*,#7675,.T.);
#10551=ORIENTED_EDGE('',*,*,#7676,.T.);
#10552=ORIENTED_EDGE('',*,*,#7677,.T.);
#10553=ORIENTED_EDGE('',*,*,#7678,.T.);
#10554=ORIENTED_EDGE('',*,*,#7679,.T.);
#10555=ORIENTED_EDGE('',*,*,#7680,.T.);
#10556=ORIENTED_EDGE('',*,*,#7681,.T.);
#10557=ORIENTED_EDGE('',*,*,#7682,.T.);
#10558=ORIENTED_EDGE('',*,*,#7683,.T.);
#10559=ORIENTED_EDGE('',*,*,#7684,.T.);
#10560=ORIENTED_EDGE('',*,*,#7685,.T.);
#10561=ORIENTED_EDGE('',*,*,#7686,.T.);
#10562=ORIENTED_EDGE('',*,*,#7687,.T.);
#10563=ORIENTED_EDGE('',*,*,#7688,.T.);
#10564=ORIENTED_EDGE('',*,*,#7689,.T.);
#10565=ORIENTED_EDGE('',*,*,#7690,.T.);
#10566=ORIENTED_EDGE('',*,*,#7691,.T.);
#10567=ORIENTED_EDGE('',*,*,#7692,.T.);
#10568=ORIENTED_EDGE('',*,*,#7693,.T.);
#10569=ORIENTED_EDGE('',*,*,#7694,.T.);
#10570=ORIENTED_EDGE('',*,*,#7695,.T.);
#10571=ORIENTED_EDGE('',*,*,#7696,.T.);
#10572=ORIENTED_EDGE('',*,*,#7697,.T.);
#10573=ORIENTED_EDGE('',*,*,#7698,.T.);
#10574=ORIENTED_EDGE('',*,*,#7699,.T.);
#10575=ORIENTED_EDGE('',*,*,#7700,.T.);
#10576=ORIENTED_EDGE('',*,*,#7701,.T.);
#10577=ORIENTED_EDGE('',*,*,#7702,.T.);
#10578=ORIENTED_EDGE('',*,*,#7703,.T.);
#10579=ORIENTED_EDGE('',*,*,#7704,.T.);
#10580=ORIENTED_EDGE('',*,*,#7705,.T.);
#10581=ORIENTED_EDGE('',*,*,#7706,.T.);
#10582=ORIENTED_EDGE('',*,*,#7707,.T.);
#10583=ORIENTED_EDGE('',*,*,#7708,.T.);
#10584=ORIENTED_EDGE('',*,*,#7709,.T.);
#10585=ORIENTED_EDGE('',*,*,#7710,.T.);
#10586=ORIENTED_EDGE('',*,*,#7711,.T.);
#10587=ORIENTED_EDGE('',*,*,#7712,.T.);
#10588=ORIENTED_EDGE('',*,*,#7713,.T.);
#10589=ORIENTED_EDGE('',*,*,#7714,.T.);
#10590=ORIENTED_EDGE('',*,*,#7715,.T.);
#10591=ORIENTED_EDGE('',*,*,#7716,.T.);
#10592=ORIENTED_EDGE('',*,*,#7717,.T.);
#10593=ORIENTED_EDGE('',*,*,#7718,.T.);
#10594=ORIENTED_EDGE('',*,*,#7719,.T.);
#10595=ORIENTED_EDGE('',*,*,#7720,.T.);
#10596=ORIENTED_EDGE('',*,*,#7721,.T.);
#10597=ORIENTED_EDGE('',*,*,#7722,.T.);
#10598=ORIENTED_EDGE('',*,*,#7723,.T.);
#10599=ORIENTED_EDGE('',*,*,#7724,.T.);
#10600=ORIENTED_EDGE('',*,*,#7725,.T.);
#10601=ORIENTED_EDGE('',*,*,#7726,.T.);
#10602=ORIENTED_EDGE('',*,*,#7727,.T.);
#10603=ORIENTED_EDGE('',*,*,#7728,.T.);
#10604=ORIENTED_EDGE('',*,*,#7729,.T.);
#10605=ORIENTED_EDGE('',*,*,#7730,.T.);
#10606=ORIENTED_EDGE('',*,*,#7731,.T.);
#10607=ORIENTED_EDGE('',*,*,#7732,.T.);
#10608=ORIENTED_EDGE('',*,*,#7733,.T.);
#10609=ORIENTED_EDGE('',*,*,#7734,.T.);
#10610=ORIENTED_EDGE('',*,*,#7735,.T.);
#10611=ORIENTED_EDGE('',*,*,#7736,.T.);
#10612=ORIENTED_EDGE('',*,*,#7737,.T.);
#10613=ORIENTED_EDGE('',*,*,#7738,.T.);
#10614=ORIENTED_EDGE('',*,*,#7739,.T.);
#10615=ORIENTED_EDGE('',*,*,#7740,.T.);
#10616=ORIENTED_EDGE('',*,*,#7741,.T.);
#10617=ORIENTED_EDGE('',*,*,#7742,.T.);
#10618=ORIENTED_EDGE('',*,*,#7743,.T.);
#10619=ORIENTED_EDGE('',*,*,#7744,.T.);
#10620=ORIENTED_EDGE('',*,*,#7745,.T.);
#10621=ORIENTED_EDGE('',*,*,#7746,.T.);
#10622=ORIENTED_EDGE('',*,*,#7747,.T.);
#10623=ORIENTED_EDGE('',*,*,#7748,.T.);
#10624=ORIENTED_EDGE('',*,*,#7749,.T.);
#10625=ORIENTED_EDGE('',*,*,#7750,.T.);
#10626=ORIENTED_EDGE('',*,*,#7751,.T.);
#10627=ORIENTED_EDGE('',*,*,#7752,.T.);
#10628=ORIENTED_EDGE('',*,*,#7753,.T.);
#10629=ORIENTED_EDGE('',*,*,#7754,.T.);
#10630=ORIENTED_EDGE('',*,*,#7755,.F.);
#10631=ORIENTED_EDGE('',*,*,#7756,.T.);
#10632=ORIENTED_EDGE('',*,*,#7674,.T.);
#10633=ORIENTED_EDGE('',*,*,#7756,.F.);
#10634=ORIENTED_EDGE('',*,*,#7755,.T.);
#10635=ORIENTED_EDGE('',*,*,#7590,.T.);
#10636=ORIENTED_EDGE('',*,*,#7757,.F.);
#10637=ORIENTED_EDGE('',*,*,#7675,.F.);
#10638=ORIENTED_EDGE('',*,*,#7758,.F.);
#10639=ORIENTED_EDGE('',*,*,#7592,.F.);
#10640=ORIENTED_EDGE('',*,*,#7758,.T.);
#10641=ORIENTED_EDGE('',*,*,#7754,.F.);
#10642=ORIENTED_EDGE('',*,*,#7759,.T.);
#10643=ORIENTED_EDGE('',*,*,#7593,.T.);
#10644=ORIENTED_EDGE('',*,*,#7759,.F.);
#10645=ORIENTED_EDGE('',*,*,#7753,.F.);
#10646=ORIENTED_EDGE('',*,*,#7760,.F.);
#10647=ORIENTED_EDGE('',*,*,#7594,.F.);
#10648=ORIENTED_EDGE('',*,*,#7760,.T.);
#10649=ORIENTED_EDGE('',*,*,#7752,.F.);
#10650=ORIENTED_EDGE('',*,*,#7761,.T.);
#10651=ORIENTED_EDGE('',*,*,#7595,.T.);
#10652=ORIENTED_EDGE('',*,*,#7761,.F.);
#10653=ORIENTED_EDGE('',*,*,#7751,.F.);
#10654=ORIENTED_EDGE('',*,*,#7762,.F.);
#10655=ORIENTED_EDGE('',*,*,#7596,.F.);
#10656=ORIENTED_EDGE('',*,*,#7762,.T.);
#10657=ORIENTED_EDGE('',*,*,#7750,.F.);
#10658=ORIENTED_EDGE('',*,*,#7763,.T.);
#10659=ORIENTED_EDGE('',*,*,#7597,.T.);
#10660=ORIENTED_EDGE('',*,*,#7763,.F.);
#10661=ORIENTED_EDGE('',*,*,#7749,.F.);
#10662=ORIENTED_EDGE('',*,*,#7764,.F.);
#10663=ORIENTED_EDGE('',*,*,#7598,.F.);
#10664=ORIENTED_EDGE('',*,*,#7764,.T.);
#10665=ORIENTED_EDGE('',*,*,#7748,.F.);
#10666=ORIENTED_EDGE('',*,*,#7765,.T.);
#10667=ORIENTED_EDGE('',*,*,#7599,.T.);
#10668=ORIENTED_EDGE('',*,*,#7765,.F.);
#10669=ORIENTED_EDGE('',*,*,#7747,.F.);
#10670=ORIENTED_EDGE('',*,*,#7766,.F.);
#10671=ORIENTED_EDGE('',*,*,#7600,.F.);
#10672=ORIENTED_EDGE('',*,*,#7766,.T.);
#10673=ORIENTED_EDGE('',*,*,#7746,.F.);
#10674=ORIENTED_EDGE('',*,*,#7767,.T.);
#10675=ORIENTED_EDGE('',*,*,#7601,.T.);
#10676=ORIENTED_EDGE('',*,*,#7767,.F.);
#10677=ORIENTED_EDGE('',*,*,#7745,.F.);
#10678=ORIENTED_EDGE('',*,*,#7768,.F.);
#10679=ORIENTED_EDGE('',*,*,#7602,.F.);
#10680=ORIENTED_EDGE('',*,*,#7768,.T.);
#10681=ORIENTED_EDGE('',*,*,#7744,.F.);
#10682=ORIENTED_EDGE('',*,*,#7769,.T.);
#10683=ORIENTED_EDGE('',*,*,#7603,.T.);
#10684=ORIENTED_EDGE('',*,*,#7769,.F.);
#10685=ORIENTED_EDGE('',*,*,#7743,.F.);
#10686=ORIENTED_EDGE('',*,*,#7770,.F.);
#10687=ORIENTED_EDGE('',*,*,#7604,.F.);
#10688=ORIENTED_EDGE('',*,*,#7770,.T.);
#10689=ORIENTED_EDGE('',*,*,#7742,.F.);
#10690=ORIENTED_EDGE('',*,*,#7771,.T.);
#10691=ORIENTED_EDGE('',*,*,#7605,.T.);
#10692=ORIENTED_EDGE('',*,*,#7771,.F.);
#10693=ORIENTED_EDGE('',*,*,#7741,.F.);
#10694=ORIENTED_EDGE('',*,*,#7772,.F.);
#10695=ORIENTED_EDGE('',*,*,#7606,.F.);
#10696=ORIENTED_EDGE('',*,*,#7772,.T.);
#10697=ORIENTED_EDGE('',*,*,#7740,.F.);
#10698=ORIENTED_EDGE('',*,*,#7773,.T.);
#10699=ORIENTED_EDGE('',*,*,#7607,.T.);
#10700=ORIENTED_EDGE('',*,*,#7773,.F.);
#10701=ORIENTED_EDGE('',*,*,#7739,.F.);
#10702=ORIENTED_EDGE('',*,*,#7774,.F.);
#10703=ORIENTED_EDGE('',*,*,#7608,.F.);
#10704=ORIENTED_EDGE('',*,*,#7774,.T.);
#10705=ORIENTED_EDGE('',*,*,#7738,.F.);
#10706=ORIENTED_EDGE('',*,*,#7775,.T.);
#10707=ORIENTED_EDGE('',*,*,#7609,.T.);
#10708=ORIENTED_EDGE('',*,*,#7775,.F.);
#10709=ORIENTED_EDGE('',*,*,#7737,.F.);
#10710=ORIENTED_EDGE('',*,*,#7776,.F.);
#10711=ORIENTED_EDGE('',*,*,#7610,.F.);
#10712=ORIENTED_EDGE('',*,*,#7776,.T.);
#10713=ORIENTED_EDGE('',*,*,#7736,.F.);
#10714=ORIENTED_EDGE('',*,*,#7777,.T.);
#10715=ORIENTED_EDGE('',*,*,#7611,.T.);
#10716=ORIENTED_EDGE('',*,*,#7777,.F.);
#10717=ORIENTED_EDGE('',*,*,#7735,.F.);
#10718=ORIENTED_EDGE('',*,*,#7778,.F.);
#10719=ORIENTED_EDGE('',*,*,#7612,.F.);
#10720=ORIENTED_EDGE('',*,*,#7778,.T.);
#10721=ORIENTED_EDGE('',*,*,#7734,.F.);
#10722=ORIENTED_EDGE('',*,*,#7779,.T.);
#10723=ORIENTED_EDGE('',*,*,#7613,.T.);
#10724=ORIENTED_EDGE('',*,*,#7779,.F.);
#10725=ORIENTED_EDGE('',*,*,#7733,.F.);
#10726=ORIENTED_EDGE('',*,*,#7780,.F.);
#10727=ORIENTED_EDGE('',*,*,#7614,.F.);
#10728=ORIENTED_EDGE('',*,*,#7780,.T.);
#10729=ORIENTED_EDGE('',*,*,#7732,.F.);
#10730=ORIENTED_EDGE('',*,*,#7781,.T.);
#10731=ORIENTED_EDGE('',*,*,#7615,.T.);
#10732=ORIENTED_EDGE('',*,*,#7781,.F.);
#10733=ORIENTED_EDGE('',*,*,#7731,.F.);
#10734=ORIENTED_EDGE('',*,*,#7782,.F.);
#10735=ORIENTED_EDGE('',*,*,#7616,.F.);
#10736=ORIENTED_EDGE('',*,*,#7782,.T.);
#10737=ORIENTED_EDGE('',*,*,#7730,.F.);
#10738=ORIENTED_EDGE('',*,*,#7783,.T.);
#10739=ORIENTED_EDGE('',*,*,#7617,.T.);
#10740=ORIENTED_EDGE('',*,*,#7783,.F.);
#10741=ORIENTED_EDGE('',*,*,#7729,.F.);
#10742=ORIENTED_EDGE('',*,*,#7784,.F.);
#10743=ORIENTED_EDGE('',*,*,#7618,.F.);
#10744=ORIENTED_EDGE('',*,*,#7784,.T.);
#10745=ORIENTED_EDGE('',*,*,#7728,.F.);
#10746=ORIENTED_EDGE('',*,*,#7785,.T.);
#10747=ORIENTED_EDGE('',*,*,#7619,.T.);
#10748=ORIENTED_EDGE('',*,*,#7785,.F.);
#10749=ORIENTED_EDGE('',*,*,#7727,.F.);
#10750=ORIENTED_EDGE('',*,*,#7786,.F.);
#10751=ORIENTED_EDGE('',*,*,#7620,.F.);
#10752=ORIENTED_EDGE('',*,*,#7786,.T.);
#10753=ORIENTED_EDGE('',*,*,#7726,.F.);
#10754=ORIENTED_EDGE('',*,*,#7787,.T.);
#10755=ORIENTED_EDGE('',*,*,#7621,.T.);
#10756=ORIENTED_EDGE('',*,*,#7787,.F.);
#10757=ORIENTED_EDGE('',*,*,#7725,.F.);
#10758=ORIENTED_EDGE('',*,*,#7788,.F.);
#10759=ORIENTED_EDGE('',*,*,#7622,.F.);
#10760=ORIENTED_EDGE('',*,*,#7788,.T.);
#10761=ORIENTED_EDGE('',*,*,#7724,.F.);
#10762=ORIENTED_EDGE('',*,*,#7789,.T.);
#10763=ORIENTED_EDGE('',*,*,#7623,.T.);
#10764=ORIENTED_EDGE('',*,*,#7789,.F.);
#10765=ORIENTED_EDGE('',*,*,#7723,.F.);
#10766=ORIENTED_EDGE('',*,*,#7790,.F.);
#10767=ORIENTED_EDGE('',*,*,#7624,.F.);
#10768=ORIENTED_EDGE('',*,*,#7790,.T.);
#10769=ORIENTED_EDGE('',*,*,#7722,.F.);
#10770=ORIENTED_EDGE('',*,*,#7791,.T.);
#10771=ORIENTED_EDGE('',*,*,#7625,.T.);
#10772=ORIENTED_EDGE('',*,*,#7791,.F.);
#10773=ORIENTED_EDGE('',*,*,#7721,.F.);
#10774=ORIENTED_EDGE('',*,*,#7792,.F.);
#10775=ORIENTED_EDGE('',*,*,#7626,.F.);
#10776=ORIENTED_EDGE('',*,*,#7792,.T.);
#10777=ORIENTED_EDGE('',*,*,#7720,.F.);
#10778=ORIENTED_EDGE('',*,*,#7793,.T.);
#10779=ORIENTED_EDGE('',*,*,#7627,.T.);
#10780=ORIENTED_EDGE('',*,*,#7793,.F.);
#10781=ORIENTED_EDGE('',*,*,#7719,.F.);
#10782=ORIENTED_EDGE('',*,*,#7794,.F.);
#10783=ORIENTED_EDGE('',*,*,#7628,.F.);
#10784=ORIENTED_EDGE('',*,*,#7794,.T.);
#10785=ORIENTED_EDGE('',*,*,#7718,.F.);
#10786=ORIENTED_EDGE('',*,*,#7795,.T.);
#10787=ORIENTED_EDGE('',*,*,#7629,.T.);
#10788=ORIENTED_EDGE('',*,*,#7795,.F.);
#10789=ORIENTED_EDGE('',*,*,#7717,.F.);
#10790=ORIENTED_EDGE('',*,*,#7796,.F.);
#10791=ORIENTED_EDGE('',*,*,#7630,.F.);
#10792=ORIENTED_EDGE('',*,*,#7796,.T.);
#10793=ORIENTED_EDGE('',*,*,#7716,.F.);
#10794=ORIENTED_EDGE('',*,*,#7797,.T.);
#10795=ORIENTED_EDGE('',*,*,#7631,.T.);
#10796=ORIENTED_EDGE('',*,*,#7797,.F.);
#10797=ORIENTED_EDGE('',*,*,#7715,.F.);
#10798=ORIENTED_EDGE('',*,*,#7798,.F.);
#10799=ORIENTED_EDGE('',*,*,#7632,.F.);
#10800=ORIENTED_EDGE('',*,*,#7798,.T.);
#10801=ORIENTED_EDGE('',*,*,#7714,.F.);
#10802=ORIENTED_EDGE('',*,*,#7799,.T.);
#10803=ORIENTED_EDGE('',*,*,#7633,.T.);
#10804=ORIENTED_EDGE('',*,*,#7799,.F.);
#10805=ORIENTED_EDGE('',*,*,#7713,.F.);
#10806=ORIENTED_EDGE('',*,*,#7800,.F.);
#10807=ORIENTED_EDGE('',*,*,#7634,.F.);
#10808=ORIENTED_EDGE('',*,*,#7800,.T.);
#10809=ORIENTED_EDGE('',*,*,#7712,.F.);
#10810=ORIENTED_EDGE('',*,*,#7801,.T.);
#10811=ORIENTED_EDGE('',*,*,#7635,.T.);
#10812=ORIENTED_EDGE('',*,*,#7801,.F.);
#10813=ORIENTED_EDGE('',*,*,#7711,.F.);
#10814=ORIENTED_EDGE('',*,*,#7802,.F.);
#10815=ORIENTED_EDGE('',*,*,#7636,.F.);
#10816=ORIENTED_EDGE('',*,*,#7802,.T.);
#10817=ORIENTED_EDGE('',*,*,#7710,.F.);
#10818=ORIENTED_EDGE('',*,*,#7803,.T.);
#10819=ORIENTED_EDGE('',*,*,#7637,.T.);
#10820=ORIENTED_EDGE('',*,*,#7803,.F.);
#10821=ORIENTED_EDGE('',*,*,#7709,.F.);
#10822=ORIENTED_EDGE('',*,*,#7804,.F.);
#10823=ORIENTED_EDGE('',*,*,#7638,.F.);
#10824=ORIENTED_EDGE('',*,*,#7804,.T.);
#10825=ORIENTED_EDGE('',*,*,#7708,.F.);
#10826=ORIENTED_EDGE('',*,*,#7805,.T.);
#10827=ORIENTED_EDGE('',*,*,#7639,.T.);
#10828=ORIENTED_EDGE('',*,*,#7805,.F.);
#10829=ORIENTED_EDGE('',*,*,#7707,.F.);
#10830=ORIENTED_EDGE('',*,*,#7806,.F.);
#10831=ORIENTED_EDGE('',*,*,#7640,.F.);
#10832=ORIENTED_EDGE('',*,*,#7806,.T.);
#10833=ORIENTED_EDGE('',*,*,#7706,.F.);
#10834=ORIENTED_EDGE('',*,*,#7807,.T.);
#10835=ORIENTED_EDGE('',*,*,#7641,.T.);
#10836=ORIENTED_EDGE('',*,*,#7807,.F.);
#10837=ORIENTED_EDGE('',*,*,#7705,.F.);
#10838=ORIENTED_EDGE('',*,*,#7808,.F.);
#10839=ORIENTED_EDGE('',*,*,#7642,.F.);
#10840=ORIENTED_EDGE('',*,*,#7808,.T.);
#10841=ORIENTED_EDGE('',*,*,#7704,.F.);
#10842=ORIENTED_EDGE('',*,*,#7809,.T.);
#10843=ORIENTED_EDGE('',*,*,#7643,.T.);
#10844=ORIENTED_EDGE('',*,*,#7809,.F.);
#10845=ORIENTED_EDGE('',*,*,#7703,.F.);
#10846=ORIENTED_EDGE('',*,*,#7810,.F.);
#10847=ORIENTED_EDGE('',*,*,#7644,.F.);
#10848=ORIENTED_EDGE('',*,*,#7810,.T.);
#10849=ORIENTED_EDGE('',*,*,#7702,.F.);
#10850=ORIENTED_EDGE('',*,*,#7811,.T.);
#10851=ORIENTED_EDGE('',*,*,#7645,.T.);
#10852=ORIENTED_EDGE('',*,*,#7811,.F.);
#10853=ORIENTED_EDGE('',*,*,#7701,.F.);
#10854=ORIENTED_EDGE('',*,*,#7812,.F.);
#10855=ORIENTED_EDGE('',*,*,#7646,.F.);
#10856=ORIENTED_EDGE('',*,*,#7812,.T.);
#10857=ORIENTED_EDGE('',*,*,#7700,.F.);
#10858=ORIENTED_EDGE('',*,*,#7813,.T.);
#10859=ORIENTED_EDGE('',*,*,#7647,.T.);
#10860=ORIENTED_EDGE('',*,*,#7813,.F.);
#10861=ORIENTED_EDGE('',*,*,#7699,.F.);
#10862=ORIENTED_EDGE('',*,*,#7814,.F.);
#10863=ORIENTED_EDGE('',*,*,#7648,.F.);
#10864=ORIENTED_EDGE('',*,*,#7814,.T.);
#10865=ORIENTED_EDGE('',*,*,#7698,.F.);
#10866=ORIENTED_EDGE('',*,*,#7815,.T.);
#10867=ORIENTED_EDGE('',*,*,#7649,.T.);
#10868=ORIENTED_EDGE('',*,*,#7815,.F.);
#10869=ORIENTED_EDGE('',*,*,#7697,.F.);
#10870=ORIENTED_EDGE('',*,*,#7816,.F.);
#10871=ORIENTED_EDGE('',*,*,#7650,.F.);
#10872=ORIENTED_EDGE('',*,*,#7816,.T.);
#10873=ORIENTED_EDGE('',*,*,#7696,.F.);
#10874=ORIENTED_EDGE('',*,*,#7817,.T.);
#10875=ORIENTED_EDGE('',*,*,#7651,.T.);
#10876=ORIENTED_EDGE('',*,*,#7817,.F.);
#10877=ORIENTED_EDGE('',*,*,#7695,.F.);
#10878=ORIENTED_EDGE('',*,*,#7818,.F.);
#10879=ORIENTED_EDGE('',*,*,#7652,.F.);
#10880=ORIENTED_EDGE('',*,*,#7818,.T.);
#10881=ORIENTED_EDGE('',*,*,#7694,.F.);
#10882=ORIENTED_EDGE('',*,*,#7819,.T.);
#10883=ORIENTED_EDGE('',*,*,#7653,.T.);
#10884=ORIENTED_EDGE('',*,*,#7819,.F.);
#10885=ORIENTED_EDGE('',*,*,#7693,.F.);
#10886=ORIENTED_EDGE('',*,*,#7820,.F.);
#10887=ORIENTED_EDGE('',*,*,#7654,.F.);
#10888=ORIENTED_EDGE('',*,*,#7820,.T.);
#10889=ORIENTED_EDGE('',*,*,#7692,.F.);
#10890=ORIENTED_EDGE('',*,*,#7821,.T.);
#10891=ORIENTED_EDGE('',*,*,#7655,.T.);
#10892=ORIENTED_EDGE('',*,*,#7821,.F.);
#10893=ORIENTED_EDGE('',*,*,#7691,.F.);
#10894=ORIENTED_EDGE('',*,*,#7822,.F.);
#10895=ORIENTED_EDGE('',*,*,#7656,.F.);
#10896=ORIENTED_EDGE('',*,*,#7822,.T.);
#10897=ORIENTED_EDGE('',*,*,#7690,.F.);
#10898=ORIENTED_EDGE('',*,*,#7823,.T.);
#10899=ORIENTED_EDGE('',*,*,#7657,.T.);
#10900=ORIENTED_EDGE('',*,*,#7823,.F.);
#10901=ORIENTED_EDGE('',*,*,#7689,.F.);
#10902=ORIENTED_EDGE('',*,*,#7824,.F.);
#10903=ORIENTED_EDGE('',*,*,#7658,.F.);
#10904=ORIENTED_EDGE('',*,*,#7824,.T.);
#10905=ORIENTED_EDGE('',*,*,#7688,.F.);
#10906=ORIENTED_EDGE('',*,*,#7825,.T.);
#10907=ORIENTED_EDGE('',*,*,#7659,.T.);
#10908=ORIENTED_EDGE('',*,*,#7825,.F.);
#10909=ORIENTED_EDGE('',*,*,#7687,.F.);
#10910=ORIENTED_EDGE('',*,*,#7826,.F.);
#10911=ORIENTED_EDGE('',*,*,#7660,.F.);
#10912=ORIENTED_EDGE('',*,*,#7826,.T.);
#10913=ORIENTED_EDGE('',*,*,#7686,.F.);
#10914=ORIENTED_EDGE('',*,*,#7827,.T.);
#10915=ORIENTED_EDGE('',*,*,#7661,.T.);
#10916=ORIENTED_EDGE('',*,*,#7827,.F.);
#10917=ORIENTED_EDGE('',*,*,#7685,.F.);
#10918=ORIENTED_EDGE('',*,*,#7828,.F.);
#10919=ORIENTED_EDGE('',*,*,#7662,.F.);
#10920=ORIENTED_EDGE('',*,*,#7828,.T.);
#10921=ORIENTED_EDGE('',*,*,#7684,.F.);
#10922=ORIENTED_EDGE('',*,*,#7829,.T.);
#10923=ORIENTED_EDGE('',*,*,#7663,.T.);
#10924=ORIENTED_EDGE('',*,*,#7829,.F.);
#10925=ORIENTED_EDGE('',*,*,#7683,.F.);
#10926=ORIENTED_EDGE('',*,*,#7830,.F.);
#10927=ORIENTED_EDGE('',*,*,#7664,.F.);
#10928=ORIENTED_EDGE('',*,*,#7830,.T.);
#10929=ORIENTED_EDGE('',*,*,#7682,.F.);
#10930=ORIENTED_EDGE('',*,*,#7831,.T.);
#10931=ORIENTED_EDGE('',*,*,#7665,.T.);
#10932=ORIENTED_EDGE('',*,*,#7831,.F.);
#10933=ORIENTED_EDGE('',*,*,#7681,.F.);
#10934=ORIENTED_EDGE('',*,*,#7832,.F.);
#10935=ORIENTED_EDGE('',*,*,#7666,.F.);
#10936=ORIENTED_EDGE('',*,*,#7832,.T.);
#10937=ORIENTED_EDGE('',*,*,#7680,.F.);
#10938=ORIENTED_EDGE('',*,*,#7833,.T.);
#10939=ORIENTED_EDGE('',*,*,#7667,.T.);
#10940=ORIENTED_EDGE('',*,*,#7834,.F.);
#10941=ORIENTED_EDGE('',*,*,#7668,.F.);
#10942=ORIENTED_EDGE('',*,*,#7833,.F.);
#10943=ORIENTED_EDGE('',*,*,#7679,.F.);
#10944=ORIENTED_EDGE('',*,*,#7757,.T.);
#10945=ORIENTED_EDGE('',*,*,#7671,.T.);
#10946=ORIENTED_EDGE('',*,*,#7835,.T.);
#10947=ORIENTED_EDGE('',*,*,#7676,.F.);
#10948=ORIENTED_EDGE('',*,*,#7836,.F.);
#10949=ORIENTED_EDGE('',*,*,#7677,.F.);
#10950=ORIENTED_EDGE('',*,*,#7835,.F.);
#10951=ORIENTED_EDGE('',*,*,#7670,.F.);
#10952=ORIENTED_EDGE('',*,*,#7834,.T.);
#10953=ORIENTED_EDGE('',*,*,#7678,.F.);
#10954=ORIENTED_EDGE('',*,*,#7836,.T.);
#10955=ORIENTED_EDGE('',*,*,#7669,.T.);
#10956=ORIENTED_EDGE('',*,*,#7837,.F.);
#10957=ORIENTED_EDGE('',*,*,#7838,.F.);
#10958=ORIENTED_EDGE('',*,*,#7839,.T.);
#10959=ORIENTED_EDGE('',*,*,#7837,.T.);
#10960=ORIENTED_EDGE('',*,*,#7839,.F.);
#10961=ORIENTED_EDGE('',*,*,#7840,.F.);
#10962=ORIENTED_EDGE('',*,*,#7841,.T.);
#10963=ORIENTED_EDGE('',*,*,#7838,.T.);
#10964=ORIENTED_EDGE('',*,*,#7841,.F.);
#10965=ORIENTED_EDGE('',*,*,#7842,.F.);
#10966=ORIENTED_EDGE('',*,*,#7843,.T.);
#10967=ORIENTED_EDGE('',*,*,#7840,.T.);
#10968=ORIENTED_EDGE('',*,*,#7843,.F.);
#10969=ORIENTED_EDGE('',*,*,#7842,.T.);
#10970=ORIENTED_EDGE('',*,*,#7844,.F.);
#10971=ORIENTED_EDGE('',*,*,#7845,.F.);
#10972=ORIENTED_EDGE('',*,*,#7846,.T.);
#10973=ORIENTED_EDGE('',*,*,#7844,.T.);
#10974=ORIENTED_EDGE('',*,*,#7846,.F.);
#10975=ORIENTED_EDGE('',*,*,#7847,.F.);
#10976=ORIENTED_EDGE('',*,*,#7848,.T.);
#10977=ORIENTED_EDGE('',*,*,#7845,.T.);
#10978=ORIENTED_EDGE('',*,*,#7848,.F.);
#10979=ORIENTED_EDGE('',*,*,#7849,.F.);
#10980=ORIENTED_EDGE('',*,*,#7850,.T.);
#10981=ORIENTED_EDGE('',*,*,#7847,.T.);
#10982=ORIENTED_EDGE('',*,*,#7850,.F.);
#10983=ORIENTED_EDGE('',*,*,#7849,.T.);
#10984=ORIENTED_EDGE('',*,*,#7851,.T.);
#10985=ORIENTED_EDGE('',*,*,#7852,.T.);
#10986=ORIENTED_EDGE('',*,*,#7853,.T.);
#10987=ORIENTED_EDGE('',*,*,#7854,.F.);
#10988=ORIENTED_EDGE('',*,*,#7855,.T.);
#10989=ORIENTED_EDGE('',*,*,#7856,.T.);
#10990=ORIENTED_EDGE('',*,*,#7857,.T.);
#10991=ORIENTED_EDGE('',*,*,#7852,.F.);
#10992=ORIENTED_EDGE('',*,*,#7858,.T.);
#10993=ORIENTED_EDGE('',*,*,#7859,.T.);
#10994=ORIENTED_EDGE('',*,*,#7860,.T.);
#10995=ORIENTED_EDGE('',*,*,#7856,.F.);
#10996=ORIENTED_EDGE('',*,*,#7861,.T.);
#10997=ORIENTED_EDGE('',*,*,#7862,.T.);
#10998=ORIENTED_EDGE('',*,*,#7863,.T.);
#10999=ORIENTED_EDGE('',*,*,#7859,.F.);
#11000=ORIENTED_EDGE('',*,*,#7864,.T.);
#11001=ORIENTED_EDGE('',*,*,#7865,.T.);
#11002=ORIENTED_EDGE('',*,*,#7866,.T.);
#11003=ORIENTED_EDGE('',*,*,#7862,.F.);
#11004=ORIENTED_EDGE('',*,*,#7867,.T.);
#11005=ORIENTED_EDGE('',*,*,#7854,.T.);
#11006=ORIENTED_EDGE('',*,*,#7868,.T.);
#11007=ORIENTED_EDGE('',*,*,#7865,.F.);
#11008=ORIENTED_EDGE('',*,*,#7867,.F.);
#11009=ORIENTED_EDGE('',*,*,#7864,.F.);
#11010=ORIENTED_EDGE('',*,*,#7861,.F.);
#11011=ORIENTED_EDGE('',*,*,#7858,.F.);
#11012=ORIENTED_EDGE('',*,*,#7855,.F.);
#11013=ORIENTED_EDGE('',*,*,#7851,.F.);
#11014=ORIENTED_EDGE('',*,*,#7868,.F.);
#11015=ORIENTED_EDGE('',*,*,#7853,.F.);
#11016=ORIENTED_EDGE('',*,*,#7857,.F.);
#11017=ORIENTED_EDGE('',*,*,#7860,.F.);
#11018=ORIENTED_EDGE('',*,*,#7863,.F.);
#11019=ORIENTED_EDGE('',*,*,#7866,.F.);
#11020=ORIENTED_EDGE('',*,*,#7869,.F.);
#11021=ORIENTED_EDGE('',*,*,#7870,.T.);
#11022=ORIENTED_EDGE('',*,*,#7871,.T.);
#11023=ORIENTED_EDGE('',*,*,#7870,.F.);
#11024=ORIENTED_EDGE('',*,*,#7871,.F.);
#11025=ORIENTED_EDGE('',*,*,#7872,.T.);
#11026=ORIENTED_EDGE('',*,*,#7873,.F.);
#11027=ORIENTED_EDGE('',*,*,#7874,.F.);
#11028=ORIENTED_EDGE('',*,*,#7875,.F.);
#11029=ORIENTED_EDGE('',*,*,#7872,.F.);
#11030=ORIENTED_EDGE('',*,*,#7876,.T.);
#11031=ORIENTED_EDGE('',*,*,#7874,.T.);
#11032=ORIENTED_EDGE('',*,*,#7876,.F.);
#11033=ORIENTED_EDGE('',*,*,#7875,.T.);
#11034=ORIENTED_EDGE('',*,*,#7877,.T.);
#11035=ORIENTED_EDGE('',*,*,#7878,.T.);
#11036=ORIENTED_EDGE('',*,*,#7877,.F.);
#11037=ORIENTED_EDGE('',*,*,#7879,.T.);
#11038=ORIENTED_EDGE('',*,*,#7880,.F.);
#11039=ORIENTED_EDGE('',*,*,#7881,.F.);
#11040=ORIENTED_EDGE('',*,*,#7882,.F.);
#11041=ORIENTED_EDGE('',*,*,#7879,.F.);
#11042=ORIENTED_EDGE('',*,*,#7883,.T.);
#11043=ORIENTED_EDGE('',*,*,#7881,.T.);
#11044=ORIENTED_EDGE('',*,*,#7883,.F.);
#11045=ORIENTED_EDGE('',*,*,#7882,.T.);
#11046=ORIENTED_EDGE('',*,*,#7884,.T.);
#11047=ORIENTED_EDGE('',*,*,#7885,.T.);
#11048=ORIENTED_EDGE('',*,*,#7884,.F.);
#11049=ORIENTED_EDGE('',*,*,#7878,.F.);
#11050=ORIENTED_EDGE('',*,*,#7886,.F.);
#11051=ORIENTED_EDGE('',*,*,#7887,.F.);
#11052=ORIENTED_EDGE('',*,*,#7888,.T.);
#11053=ORIENTED_EDGE('',*,*,#7873,.T.);
#11054=ORIENTED_EDGE('',*,*,#7888,.F.);
#11055=ORIENTED_EDGE('',*,*,#7889,.T.);
#11056=ORIENTED_EDGE('',*,*,#7890,.F.);
#11057=ORIENTED_EDGE('',*,*,#7889,.F.);
#11058=ORIENTED_EDGE('',*,*,#7891,.T.);
#11059=ORIENTED_EDGE('',*,*,#7880,.T.);
#11060=ORIENTED_EDGE('',*,*,#7891,.F.);
#11061=ORIENTED_EDGE('',*,*,#7886,.T.);
#11062=ORIENTED_EDGE('',*,*,#7892,.T.);
#11063=ORIENTED_EDGE('',*,*,#7890,.T.);
#11064=ORIENTED_EDGE('',*,*,#7892,.F.);
#11065=ORIENTED_EDGE('',*,*,#7887,.T.);
#11066=ORIENTED_EDGE('',*,*,#7885,.F.);
#11067=ORIENTED_EDGE('',*,*,#7869,.T.);
#11068=ORIENTED_EDGE('',*,*,#7893,.F.);
#11069=ORIENTED_EDGE('',*,*,#7894,.T.);
#11070=ORIENTED_EDGE('',*,*,#7895,.F.);
#11071=ORIENTED_EDGE('',*,*,#7896,.F.);
#11072=ORIENTED_EDGE('',*,*,#7897,.F.);
#11073=ORIENTED_EDGE('',*,*,#7898,.F.);
#11074=ORIENTED_EDGE('',*,*,#7894,.F.);
#11075=ORIENTED_EDGE('',*,*,#7899,.F.);
#11076=ORIENTED_EDGE('',*,*,#7900,.T.);
#11077=ORIENTED_EDGE('',*,*,#7901,.F.);
#11078=ORIENTED_EDGE('',*,*,#7902,.F.);
#11079=ORIENTED_EDGE('',*,*,#7903,.F.);
#11080=ORIENTED_EDGE('',*,*,#7900,.F.);
#11081=ORIENTED_EDGE('',*,*,#7904,.F.);
#11082=ORIENTED_EDGE('',*,*,#7896,.T.);
#11083=ORIENTED_EDGE('',*,*,#7905,.F.);
#11084=ORIENTED_EDGE('',*,*,#7906,.T.);
#11085=ORIENTED_EDGE('',*,*,#7897,.T.);
#11086=ORIENTED_EDGE('',*,*,#7904,.T.);
#11087=ORIENTED_EDGE('',*,*,#7895,.T.);
#11088=ORIENTED_EDGE('',*,*,#7907,.T.);
#11089=ORIENTED_EDGE('',*,*,#7908,.T.);
#11090=ORIENTED_EDGE('',*,*,#7907,.F.);
#11091=ORIENTED_EDGE('',*,*,#7899,.T.);
#11092=ORIENTED_EDGE('',*,*,#7893,.T.);
#11093=ORIENTED_EDGE('',*,*,#7898,.T.);
#11094=ORIENTED_EDGE('',*,*,#7906,.F.);
#11095=ORIENTED_EDGE('',*,*,#7909,.F.);
#11096=ORIENTED_EDGE('',*,*,#7910,.T.);
#11097=ORIENTED_EDGE('',*,*,#7902,.T.);
#11098=ORIENTED_EDGE('',*,*,#7901,.T.);
#11099=ORIENTED_EDGE('',*,*,#7911,.T.);
#11100=ORIENTED_EDGE('',*,*,#7912,.T.);
#11101=ORIENTED_EDGE('',*,*,#7911,.F.);
#11102=ORIENTED_EDGE('',*,*,#7903,.T.);
#11103=ORIENTED_EDGE('',*,*,#7910,.F.);
#11104=ORIENTED_EDGE('',*,*,#7909,.T.);
#11105=ORIENTED_EDGE('',*,*,#7905,.T.);
#11106=ORIENTED_EDGE('',*,*,#7912,.F.);
#11107=ORIENTED_EDGE('',*,*,#7908,.F.);
#11108=ORIENTED_EDGE('',*,*,#7913,.F.);
#11109=ORIENTED_EDGE('',*,*,#7914,.T.);
#11110=ORIENTED_EDGE('',*,*,#7915,.T.);
#11111=ORIENTED_EDGE('',*,*,#7916,.F.);
#11112=ORIENTED_EDGE('',*,*,#7917,.F.);
#11113=ORIENTED_EDGE('',*,*,#7918,.T.);
#11114=ORIENTED_EDGE('',*,*,#7919,.T.);
#11115=ORIENTED_EDGE('',*,*,#7914,.F.);
#11116=ORIENTED_EDGE('',*,*,#7920,.F.);
#11117=ORIENTED_EDGE('',*,*,#7921,.T.);
#11118=ORIENTED_EDGE('',*,*,#7922,.T.);
#11119=ORIENTED_EDGE('',*,*,#7918,.F.);
#11120=ORIENTED_EDGE('',*,*,#7923,.F.);
#11121=ORIENTED_EDGE('',*,*,#7924,.T.);
#11122=ORIENTED_EDGE('',*,*,#7925,.T.);
#11123=ORIENTED_EDGE('',*,*,#7921,.F.);
#11124=ORIENTED_EDGE('',*,*,#7926,.F.);
#11125=ORIENTED_EDGE('',*,*,#7927,.T.);
#11126=ORIENTED_EDGE('',*,*,#7928,.T.);
#11127=ORIENTED_EDGE('',*,*,#7924,.F.);
#11128=ORIENTED_EDGE('',*,*,#7929,.F.);
#11129=ORIENTED_EDGE('',*,*,#7916,.T.);
#11130=ORIENTED_EDGE('',*,*,#7930,.T.);
#11131=ORIENTED_EDGE('',*,*,#7927,.F.);
#11132=ORIENTED_EDGE('',*,*,#7930,.F.);
#11133=ORIENTED_EDGE('',*,*,#7915,.F.);
#11134=ORIENTED_EDGE('',*,*,#7919,.F.);
#11135=ORIENTED_EDGE('',*,*,#7922,.F.);
#11136=ORIENTED_EDGE('',*,*,#7925,.F.);
#11137=ORIENTED_EDGE('',*,*,#7928,.F.);
#11138=ORIENTED_EDGE('',*,*,#7931,.F.);
#11139=ORIENTED_EDGE('',*,*,#7913,.T.);
#11140=ORIENTED_EDGE('',*,*,#7929,.T.);
#11141=ORIENTED_EDGE('',*,*,#7926,.T.);
#11142=ORIENTED_EDGE('',*,*,#7923,.T.);
#11143=ORIENTED_EDGE('',*,*,#7920,.T.);
#11144=ORIENTED_EDGE('',*,*,#7917,.T.);
#11145=ORIENTED_EDGE('',*,*,#7932,.F.);
#11146=ORIENTED_EDGE('',*,*,#7933,.T.);
#11147=ORIENTED_EDGE('',*,*,#7931,.T.);
#11148=ORIENTED_EDGE('',*,*,#7933,.F.);
#11149=ORIENTED_EDGE('',*,*,#7934,.F.);
#11150=ORIENTED_EDGE('',*,*,#7935,.T.);
#11151=ORIENTED_EDGE('',*,*,#7932,.T.);
#11152=ORIENTED_EDGE('',*,*,#7935,.F.);
#11153=ORIENTED_EDGE('',*,*,#7936,.F.);
#11154=ORIENTED_EDGE('',*,*,#7937,.T.);
#11155=ORIENTED_EDGE('',*,*,#7934,.T.);
#11156=ORIENTED_EDGE('',*,*,#7937,.F.);
#11157=ORIENTED_EDGE('',*,*,#7936,.T.);
#11158=CYLINDRICAL_SURFACE('',#12879,0.165);
#11159=CYLINDRICAL_SURFACE('',#12883,0.165);
#11160=CYLINDRICAL_SURFACE('',#12887,0.164999999999999);
#11161=CYLINDRICAL_SURFACE('',#12891,0.164999999999999);
#11162=CYLINDRICAL_SURFACE('',#12895,0.165);
#11163=CYLINDRICAL_SURFACE('',#12899,0.165);
#11164=CYLINDRICAL_SURFACE('',#12903,0.165);
#11165=CYLINDRICAL_SURFACE('',#12907,0.165);
#11166=CYLINDRICAL_SURFACE('',#12911,0.165);
#11167=CYLINDRICAL_SURFACE('',#12915,0.165);
#11168=CYLINDRICAL_SURFACE('',#12919,0.164999999999999);
#11169=CYLINDRICAL_SURFACE('',#12923,0.164999999999999);
#11170=CYLINDRICAL_SURFACE('',#12927,0.165);
#11171=CYLINDRICAL_SURFACE('',#12931,0.164999999999999);
#11172=CYLINDRICAL_SURFACE('',#12956,0.165);
#11173=CYLINDRICAL_SURFACE('',#12959,0.165);
#11174=CYLINDRICAL_SURFACE('',#12962,0.165);
#11175=CYLINDRICAL_SURFACE('',#12965,0.165);
#11176=CYLINDRICAL_SURFACE('',#12968,1.5);
#11177=CYLINDRICAL_SURFACE('',#12971,0.225);
#11178=CYLINDRICAL_SURFACE('',#12974,0.225);
#11179=CYLINDRICAL_SURFACE('',#12977,0.225);
#11180=CYLINDRICAL_SURFACE('',#12980,0.225);
#11181=CYLINDRICAL_SURFACE('',#12994,1.1);
#11182=CYLINDRICAL_SURFACE('',#12997,1.49);
#11183=CYLINDRICAL_SURFACE('',#13003,0.225);
#11184=CYLINDRICAL_SURFACE('',#13006,0.225);
#11185=CYLINDRICAL_SURFACE('',#13009,0.225);
#11186=CYLINDRICAL_SURFACE('',#13012,0.225);
#11187=CYLINDRICAL_SURFACE('',#13021,2.1);
#11188=CYLINDRICAL_SURFACE('',#13023,2.1);
#11189=CYLINDRICAL_SURFACE('',#13025,2.1);
#11190=CYLINDRICAL_SURFACE('',#13027,2.1);
#11191=CYLINDRICAL_SURFACE('',#13029,1.49);
#11192=CYLINDRICAL_SURFACE('',#13034,1.1);
#11193=CYLINDRICAL_SURFACE('',#13037,0.225);
#11194=CYLINDRICAL_SURFACE('',#13040,0.225);
#11195=CYLINDRICAL_SURFACE('',#13043,0.225);
#11196=CYLINDRICAL_SURFACE('',#13046,0.225);
#11197=CYLINDRICAL_SURFACE('',#13055,2.1);
#11198=CYLINDRICAL_SURFACE('',#13057,2.1);
#11199=CYLINDRICAL_SURFACE('',#13059,2.1);
#11200=CYLINDRICAL_SURFACE('',#13061,2.1);
#11201=CYLINDRICAL_SURFACE('',#13063,1.49);
#11202=CYLINDRICAL_SURFACE('',#13067,1.1);
#11203=CYLINDRICAL_SURFACE('',#13071,0.4);
#11204=CYLINDRICAL_SURFACE('',#13076,0.4);
#11205=CYLINDRICAL_SURFACE('',#13081,0.225);
#11206=CYLINDRICAL_SURFACE('',#13083,0.225);
#11207=CYLINDRICAL_SURFACE('',#13085,0.8);
#11208=CYLINDRICAL_SURFACE('',#13095,0.605);
#11209=CYLINDRICAL_SURFACE('',#13098,0.8);
#11210=CYLINDRICAL_SURFACE('',#13104,0.399999999999999);
#11211=CYLINDRICAL_SURFACE('',#13109,0.399999999999999);
#11212=CYLINDRICAL_SURFACE('',#13114,0.225000000000001);
#11213=CYLINDRICAL_SURFACE('',#13116,0.225000000000001);
#11214=CYLINDRICAL_SURFACE('',#13118,0.8);
#11215=CYLINDRICAL_SURFACE('',#13128,0.605);
#11216=CYLINDRICAL_SURFACE('',#13131,0.8);
#11217=CYLINDRICAL_SURFACE('',#13137,0.31);
#11218=CYLINDRICAL_SURFACE('',#13140,0.8);
#11219=CYLINDRICAL_SURFACE('',#13146,0.4);
#11220=CYLINDRICAL_SURFACE('',#13149,0.4);
#11221=CYLINDRICAL_SURFACE('',#13152,0.4);
#11222=CYLINDRICAL_SURFACE('',#13157,0.4);
#11223=CYLINDRICAL_SURFACE('',#13165,0.225);
#11224=CYLINDRICAL_SURFACE('',#13167,0.225);
#11225=CYLINDRICAL_SURFACE('',#13169,0.8);
#11226=CYLINDRICAL_SURFACE('',#13179,0.375);
#11227=CYLINDRICAL_SURFACE('',#13184,0.375);
#11228=CYLINDRICAL_SURFACE('',#13189,0.375);
#11229=CYLINDRICAL_SURFACE('',#13194,0.375);
#11230=CYLINDRICAL_SURFACE('',#13199,0.225);
#11231=CYLINDRICAL_SURFACE('',#13201,0.225);
#11232=CYLINDRICAL_SURFACE('',#13203,0.225);
#11233=CYLINDRICAL_SURFACE('',#13205,0.225000000000001);
#11234=CYLINDRICAL_SURFACE('',#13229,0.976185);
#11235=CYLINDRICAL_SURFACE('',#13231,0.5);
#11236=CYLINDRICAL_SURFACE('',#13237,0.976185);
#11237=CYLINDRICAL_SURFACE('',#13249,1.023815);
#11238=CYLINDRICAL_SURFACE('',#13256,1.5);
#11239=CYLINDRICAL_SURFACE('',#13261,1.023815);
#11240=CYLINDRICAL_SURFACE('',#13283,1.019052);
#11241=CYLINDRICAL_SURFACE('',#13323,0.980948);
#11242=CYLINDRICAL_SURFACE('',#13337,1.013815);
#11243=CYLINDRICAL_SURFACE('',#13341,0.991185);
#11244=CYLINDRICAL_SURFACE('',#13345,1.013815);
#11245=CYLINDRICAL_SURFACE('',#13349,0.991185);
#11246=CYLINDRICAL_SURFACE('',#13357,0.225);
#11247=CYLINDRICAL_SURFACE('',#13360,0.225);
#11248=CYLINDRICAL_SURFACE('',#13363,0.164999999999999);
#11249=CYLINDRICAL_SURFACE('',#13366,0.165);
#11250=CYLINDRICAL_SURFACE('',#13369,0.165);
#11251=CYLINDRICAL_SURFACE('',#13372,0.164999999999999);
#11252=CYLINDRICAL_SURFACE('',#13375,0.275);
#11253=CYLINDRICAL_SURFACE('',#13378,0.275);
#11254=CYLINDRICAL_SURFACE('',#13381,0.275);
#11255=CYLINDRICAL_SURFACE('',#13384,0.275);
#11256=CYLINDRICAL_SURFACE('',#13394,0.164999999999999);
#11257=CYLINDRICAL_SURFACE('',#13397,0.164999999999999);
#11258=CYLINDRICAL_SURFACE('',#13400,0.164999999999999);
#11259=CYLINDRICAL_SURFACE('',#13403,0.164999999999999);
#11260=CYLINDRICAL_SURFACE('',#13406,1.6);
#11261=CYLINDRICAL_SURFACE('',#13411,0.525);
#11262=CYLINDRICAL_SURFACE('',#13415,0.525);
#11263=CYLINDRICAL_SURFACE('',#13419,0.525);
#11264=CYLINDRICAL_SURFACE('',#13423,0.525);
#11265=CYLINDRICAL_SURFACE('',#13427,0.225);
#11266=CYLINDRICAL_SURFACE('',#13430,0.225);
#11267=CYLINDRICAL_SURFACE('',#13433,0.225);
#11268=CYLINDRICAL_SURFACE('',#13436,0.225);
#11269=CYLINDRICAL_SURFACE('',#13448,1.2);
#11270=CYLINDRICAL_SURFACE('',#13451,1.59);
#11271=CYLINDRICAL_SURFACE('',#13457,0.225);
#11272=CYLINDRICAL_SURFACE('',#13460,0.225);
#11273=CYLINDRICAL_SURFACE('',#13463,0.225);
#11274=CYLINDRICAL_SURFACE('',#13466,0.225);
#11275=CYLINDRICAL_SURFACE('',#13475,2.2);
#11276=CYLINDRICAL_SURFACE('',#13477,2.2);
#11277=CYLINDRICAL_SURFACE('',#13479,2.2);
#11278=CYLINDRICAL_SURFACE('',#13481,2.2);
#11279=CYLINDRICAL_SURFACE('',#13483,1.59);
#11280=CYLINDRICAL_SURFACE('',#13488,1.2);
#11281=CYLINDRICAL_SURFACE('',#13491,0.225);
#11282=CYLINDRICAL_SURFACE('',#13494,0.225);
#11283=CYLINDRICAL_SURFACE('',#13497,0.225);
#11284=CYLINDRICAL_SURFACE('',#13500,0.225);
#11285=CYLINDRICAL_SURFACE('',#13509,2.2);
#11286=CYLINDRICAL_SURFACE('',#13511,2.2);
#11287=CYLINDRICAL_SURFACE('',#13513,2.2);
#11288=CYLINDRICAL_SURFACE('',#13515,2.2);
#11289=CYLINDRICAL_SURFACE('',#13517,1.59);
#11290=CYLINDRICAL_SURFACE('',#13521,1.2);
#11291=CYLINDRICAL_SURFACE('',#13525,0.164999999999999);
#11292=CYLINDRICAL_SURFACE('',#13529,0.164999999999999);
#11293=CYLINDRICAL_SURFACE('',#13533,0.34);
#11294=CYLINDRICAL_SURFACE('',#13545,0.3);
#11295=CYLINDRICAL_SURFACE('',#13551,0.164999999999999);
#11296=CYLINDRICAL_SURFACE('',#13555,0.3);
#11297=CYLINDRICAL_SURFACE('',#13568,0.21);
#11298=CYLINDRICAL_SURFACE('',#13574,0.21);
#11299=CYLINDRICAL_SURFACE('',#13580,0.21);
#11300=CYLINDRICAL_SURFACE('',#13586,0.21);
#11301=CYLINDRICAL_SURFACE('',#13644,0.425);
#11302=CYLINDRICAL_SURFACE('',#13652,0.24505);
#11303=CYLINDRICAL_SURFACE('',#13661,1.070235);
#11304=CYLINDRICAL_SURFACE('',#13663,0.6);
#11305=CYLINDRICAL_SURFACE('',#13669,1.070235);
#11306=CYLINDRICAL_SURFACE('',#13681,1.129765);
#11307=CYLINDRICAL_SURFACE('',#13688,1.6);
#11308=CYLINDRICAL_SURFACE('',#13693,1.129765);
#11309=CYLINDRICAL_SURFACE('',#13713,1.123812);
#11310=CYLINDRICAL_SURFACE('',#13749,1.076188);
#11311=CYLINDRICAL_SURFACE('',#13763,1.119765);
#11312=CYLINDRICAL_SURFACE('',#13767,1.085235);
#11313=CYLINDRICAL_SURFACE('',#13771,1.119765);
#11314=CYLINDRICAL_SURFACE('',#13775,1.085235);
#11315=CYLINDRICAL_SURFACE('',#13796,0.35);
#11316=CYLINDRICAL_SURFACE('',#13804,0.1954);
#11317=CYLINDRICAL_SURFACE('',#13807,0.165);
#11318=CYLINDRICAL_SURFACE('',#13817,0.7);
#11319=CYLINDRICAL_SURFACE('',#13818,0.5);
#11320=CYLINDRICAL_SURFACE('',#13820,0.4);
#11321=CYLINDRICAL_SURFACE('',#13824,0.5);
#11322=CYLINDRICAL_SURFACE('',#13829,0.505);
#11323=CYLINDRICAL_SURFACE('',#13834,0.405);
#11324=CYLINDRICAL_SURFACE('',#13836,0.7);
#11325=CYLINDRICAL_SURFACE('',#13842,0.505);
#11326=CYLINDRICAL_SURFACE('',#13845,0.7);
#11327=CYLINDRICAL_SURFACE('',#13851,0.15);
#11328=CYLINDRICAL_SURFACE('',#13857,0.15);
#11329=CYLINDRICAL_SURFACE('',#13863,0.225);
#11330=CYLINDRICAL_SURFACE('',#13866,0.6);
#11331=CYLINDRICAL_SURFACE('',#13872,0.125);
#11332=CYLINDRICAL_SURFACE('',#13873,0.125);
#11333=CYLINDRICAL_SURFACE('',#13874,0.65);
#11334=CYLINDRICAL_SURFACE('',#13877,0.125);
#11335=CYLINDRICAL_SURFACE('',#13878,0.125);
#11336=CYLINDRICAL_SURFACE('',#13879,0.4);
#11337=CYLINDRICAL_SURFACE('',#13925,0.8);
#11338=CYLINDRICAL_SURFACE('',#13970,0.8);
#11339=CYLINDRICAL_SURFACE('',#13973,0.0555);
#11340=CYLINDRICAL_SURFACE('',#13974,0.611219772367581);
#11341=CYLINDRICAL_SURFACE('',#13975,0.0555);
#11342=CYLINDRICAL_SURFACE('',#13976,0.611219772367581);
#11343=CYLINDRICAL_SURFACE('',#13977,0.0555);
#11344=CYLINDRICAL_SURFACE('',#13978,0.611219772367581);
#11345=CYLINDRICAL_SURFACE('',#13979,0.0555);
#11346=CYLINDRICAL_SURFACE('',#13980,0.611219772367581);
#11347=CYLINDRICAL_SURFACE('',#13981,0.0555);
#11348=CYLINDRICAL_SURFACE('',#13982,0.611219772367581);
#11349=CYLINDRICAL_SURFACE('',#13983,0.0555);
#11350=CYLINDRICAL_SURFACE('',#13984,0.611219772367581);
#11351=CYLINDRICAL_SURFACE('',#13985,0.0555);
#11352=CYLINDRICAL_SURFACE('',#13986,0.611219772367581);
#11353=CYLINDRICAL_SURFACE('',#13987,0.0555);
#11354=CYLINDRICAL_SURFACE('',#13988,0.611219772367581);
#11355=CYLINDRICAL_SURFACE('',#13989,0.0555);
#11356=CYLINDRICAL_SURFACE('',#13990,0.611219772367581);
#11357=CYLINDRICAL_SURFACE('',#13991,0.0555);
#11358=CYLINDRICAL_SURFACE('',#13992,0.611219772367581);
#11359=CYLINDRICAL_SURFACE('',#13993,0.0555);
#11360=CYLINDRICAL_SURFACE('',#13994,0.611219772367581);
#11361=CYLINDRICAL_SURFACE('',#13995,0.0555);
#11362=CYLINDRICAL_SURFACE('',#13996,0.611219772367581);
#11363=CYLINDRICAL_SURFACE('',#13997,0.0555);
#11364=CYLINDRICAL_SURFACE('',#13998,0.611219772367581);
#11365=CYLINDRICAL_SURFACE('',#13999,0.0555);
#11366=CYLINDRICAL_SURFACE('',#14000,0.611219772367581);
#11367=CYLINDRICAL_SURFACE('',#14001,0.0555);
#11368=CYLINDRICAL_SURFACE('',#14002,0.611219772367581);
#11369=CYLINDRICAL_SURFACE('',#14003,0.0555);
#11370=CYLINDRICAL_SURFACE('',#14004,0.611219772367581);
#11371=CYLINDRICAL_SURFACE('',#14005,0.0555);
#11372=CYLINDRICAL_SURFACE('',#14006,0.611219772367581);
#11373=CYLINDRICAL_SURFACE('',#14007,0.0555);
#11374=CYLINDRICAL_SURFACE('',#14008,0.611219772367581);
#11375=CYLINDRICAL_SURFACE('',#14009,0.0555);
#11376=CYLINDRICAL_SURFACE('',#14010,0.611219772367581);
#11377=CYLINDRICAL_SURFACE('',#14011,0.0555);
#11378=CYLINDRICAL_SURFACE('',#14012,0.611219772367581);
#11379=CYLINDRICAL_SURFACE('',#14015,0.164999999999999);
#11380=CYLINDRICAL_SURFACE('',#14025,0.800000000000001);
#11381=CYLINDRICAL_SURFACE('',#14026,0.6);
#11382=CYLINDRICAL_SURFACE('',#14029,0.6);
#11383=CYLINDRICAL_SURFACE('',#14033,0.605);
#11384=CYLINDRICAL_SURFACE('',#14036,0.800000000000001);
#11385=CYLINDRICAL_SURFACE('',#14042,0.605);
#11386=CYLINDRICAL_SURFACE('',#14045,0.800000000000001);
#11387=CYLINDRICAL_SURFACE('',#14051,0.15);
#11388=CYLINDRICAL_SURFACE('',#14057,0.15);
#11389=CYLINDRICAL_SURFACE('',#14063,0.225);
#11390=CYLINDRICAL_SURFACE('',#14066,0.800000000000001);
#11391=CYLINDRICAL_SURFACE('',#14072,0.125);
#11392=CYLINDRICAL_SURFACE('',#14073,0.125);
#11393=CYLINDRICAL_SURFACE('',#14074,1.);
#11394=CYLINDRICAL_SURFACE('',#14077,0.125);
#11395=CYLINDRICAL_SURFACE('',#14078,0.125);
#11396=CYLINDRICAL_SURFACE('',#14079,0.6);
#11397=CYLINDRICAL_SURFACE('',#14165,1.4);
#11398=CYLINDRICAL_SURFACE('',#14250,1.4);
#11399=CYLINDRICAL_SURFACE('',#14253,0.0555000000000001);
#11400=CYLINDRICAL_SURFACE('',#14254,1.24783954473516);
#11401=CYLINDRICAL_SURFACE('',#14255,0.0555000000000001);
#11402=CYLINDRICAL_SURFACE('',#14256,1.24783954473516);
#11403=CYLINDRICAL_SURFACE('',#14257,0.0555000000000001);
#11404=CYLINDRICAL_SURFACE('',#14258,1.24783954473516);
#11405=CYLINDRICAL_SURFACE('',#14259,0.0555000000000001);
#11406=CYLINDRICAL_SURFACE('',#14260,1.24783954473516);
#11407=CYLINDRICAL_SURFACE('',#14261,0.0555000000000001);
#11408=CYLINDRICAL_SURFACE('',#14262,1.24783954473516);
#11409=CYLINDRICAL_SURFACE('',#14263,0.0555000000000001);
#11410=CYLINDRICAL_SURFACE('',#14264,1.24783954473516);
#11411=CYLINDRICAL_SURFACE('',#14265,0.0555000000000001);
#11412=CYLINDRICAL_SURFACE('',#14266,1.24783954473516);
#11413=CYLINDRICAL_SURFACE('',#14267,0.0555000000000001);
#11414=CYLINDRICAL_SURFACE('',#14268,1.24783954473516);
#11415=CYLINDRICAL_SURFACE('',#14269,0.0555000000000001);
#11416=CYLINDRICAL_SURFACE('',#14270,1.24783954473516);
#11417=CYLINDRICAL_SURFACE('',#14271,0.0555000000000001);
#11418=CYLINDRICAL_SURFACE('',#14272,1.24783954473516);
#11419=CYLINDRICAL_SURFACE('',#14273,0.0555000000000001);
#11420=CYLINDRICAL_SURFACE('',#14274,1.24783954473516);
#11421=CYLINDRICAL_SURFACE('',#14275,0.0555000000000001);
#11422=CYLINDRICAL_SURFACE('',#14276,1.24783954473516);
#11423=CYLINDRICAL_SURFACE('',#14277,0.0555000000000001);
#11424=CYLINDRICAL_SURFACE('',#14278,1.24783954473516);
#11425=CYLINDRICAL_SURFACE('',#14279,0.0555000000000001);
#11426=CYLINDRICAL_SURFACE('',#14280,1.24783954473516);
#11427=CYLINDRICAL_SURFACE('',#14281,0.0555000000000001);
#11428=CYLINDRICAL_SURFACE('',#14282,1.24783954473516);
#11429=CYLINDRICAL_SURFACE('',#14283,0.0555000000000001);
#11430=CYLINDRICAL_SURFACE('',#14284,1.24783954473516);
#11431=CYLINDRICAL_SURFACE('',#14285,0.0555000000000001);
#11432=CYLINDRICAL_SURFACE('',#14286,1.24783954473516);
#11433=CYLINDRICAL_SURFACE('',#14287,0.0555000000000001);
#11434=CYLINDRICAL_SURFACE('',#14288,1.24783954473516);
#11435=CYLINDRICAL_SURFACE('',#14289,0.0555000000000001);
#11436=CYLINDRICAL_SURFACE('',#14290,1.24783954473516);
#11437=CYLINDRICAL_SURFACE('',#14291,0.0555000000000001);
#11438=CYLINDRICAL_SURFACE('',#14292,1.24783954473516);
#11439=CYLINDRICAL_SURFACE('',#14293,0.0555000000000001);
#11440=CYLINDRICAL_SURFACE('',#14294,1.24783954473516);
#11441=CYLINDRICAL_SURFACE('',#14295,0.0555000000000001);
#11442=CYLINDRICAL_SURFACE('',#14296,1.24783954473516);
#11443=CYLINDRICAL_SURFACE('',#14297,0.0555000000000001);
#11444=CYLINDRICAL_SURFACE('',#14298,1.24783954473516);
#11445=CYLINDRICAL_SURFACE('',#14299,0.0555000000000001);
#11446=CYLINDRICAL_SURFACE('',#14300,1.24783954473516);
#11447=CYLINDRICAL_SURFACE('',#14301,0.0555000000000001);
#11448=CYLINDRICAL_SURFACE('',#14302,1.24783954473516);
#11449=CYLINDRICAL_SURFACE('',#14303,0.0555000000000001);
#11450=CYLINDRICAL_SURFACE('',#14304,1.24783954473516);
#11451=CYLINDRICAL_SURFACE('',#14305,0.0555000000000001);
#11452=CYLINDRICAL_SURFACE('',#14306,1.24783954473516);
#11453=CYLINDRICAL_SURFACE('',#14307,0.0555000000000001);
#11454=CYLINDRICAL_SURFACE('',#14308,1.24783954473516);
#11455=CYLINDRICAL_SURFACE('',#14309,0.0555000000000001);
#11456=CYLINDRICAL_SURFACE('',#14310,1.24783954473516);
#11457=CYLINDRICAL_SURFACE('',#14311,0.0555000000000001);
#11458=CYLINDRICAL_SURFACE('',#14312,1.24783954473516);
#11459=CYLINDRICAL_SURFACE('',#14313,0.0555000000000001);
#11460=CYLINDRICAL_SURFACE('',#14314,1.24783954473516);
#11461=CYLINDRICAL_SURFACE('',#14315,0.0555000000000001);
#11462=CYLINDRICAL_SURFACE('',#14316,1.24783954473516);
#11463=CYLINDRICAL_SURFACE('',#14317,0.0555000000000001);
#11464=CYLINDRICAL_SURFACE('',#14318,1.24783954473516);
#11465=CYLINDRICAL_SURFACE('',#14319,0.0555000000000001);
#11466=CYLINDRICAL_SURFACE('',#14320,1.24783954473516);
#11467=CYLINDRICAL_SURFACE('',#14321,0.0555000000000001);
#11468=CYLINDRICAL_SURFACE('',#14322,1.24783954473516);
#11469=CYLINDRICAL_SURFACE('',#14323,0.0555000000000001);
#11470=CYLINDRICAL_SURFACE('',#14324,1.24783954473516);
#11471=CYLINDRICAL_SURFACE('',#14325,0.0555000000000001);
#11472=CYLINDRICAL_SURFACE('',#14326,1.24783954473516);
#11473=CYLINDRICAL_SURFACE('',#14327,0.0555000000000001);
#11474=CYLINDRICAL_SURFACE('',#14328,1.24783954473516);
#11475=CYLINDRICAL_SURFACE('',#14329,0.0555000000000001);
#11476=CYLINDRICAL_SURFACE('',#14330,1.24783954473516);
#11477=CYLINDRICAL_SURFACE('',#14331,0.0555000000000001);
#11478=CYLINDRICAL_SURFACE('',#14332,1.24783954473516);
#11479=CYLINDRICAL_SURFACE('',#14338,0.35);
#11480=CYLINDRICAL_SURFACE('',#14346,0.1954);
#11481=CYLINDRICAL_SURFACE('',#14415,0.4);
#11482=CYLINDRICAL_SURFACE('',#14425,0.9);
#11483=CYLINDRICAL_SURFACE('',#14426,0.6);
#11484=CYLINDRICAL_SURFACE('',#14434,0.9);
#11485=CYLINDRICAL_SURFACE('',#14435,0.6);
#11486=CYLINDRICAL_SURFACE('',#14439,0.6);
#11487=CYLINDRICAL_SURFACE('',#14444,0.6);
#11488=CYLINDRICAL_SURFACE('',#14445,0.4);
#11489=CYLINDRICAL_SURFACE('',#14451,0.165);
#11490=CYLINDRICAL_SURFACE('',#14454,0.4);
#11491=CYLINDRICAL_SURFACE('',#14457,1.5);
#11492=CYLINDRICAL_SURFACE('',#14474,0.1954);
#11493=ADVANCED_FACE('',(#1352),#11158,.F.);
#11494=ADVANCED_FACE('',(#1353),#1037,.T.);
#11495=ADVANCED_FACE('',(#1354),#11159,.F.);
#11496=ADVANCED_FACE('',(#1355),#1038,.T.);
#11497=ADVANCED_FACE('',(#1356),#11160,.F.);
#11498=ADVANCED_FACE('',(#1357),#1039,.T.);
#11499=ADVANCED_FACE('',(#1358),#11161,.F.);
#11500=ADVANCED_FACE('',(#1359),#1040,.T.);
#11501=ADVANCED_FACE('',(#1360),#11162,.F.);
#11502=ADVANCED_FACE('',(#1361),#1041,.T.);
#11503=ADVANCED_FACE('',(#1362),#11163,.F.);
#11504=ADVANCED_FACE('',(#1363),#1042,.T.);
#11505=ADVANCED_FACE('',(#1364),#11164,.F.);
#11506=ADVANCED_FACE('',(#1365),#1043,.T.);
#11507=ADVANCED_FACE('',(#1366),#11165,.F.);
#11508=ADVANCED_FACE('',(#1367),#1044,.T.);
#11509=ADVANCED_FACE('',(#1368),#11166,.F.);
#11510=ADVANCED_FACE('',(#1369),#1045,.T.);
#11511=ADVANCED_FACE('',(#1370),#11167,.F.);
#11512=ADVANCED_FACE('',(#1371),#1046,.T.);
#11513=ADVANCED_FACE('',(#1372),#11168,.F.);
#11514=ADVANCED_FACE('',(#1373),#1047,.T.);
#11515=ADVANCED_FACE('',(#1374),#11169,.F.);
#11516=ADVANCED_FACE('',(#1375),#1048,.T.);
#11517=ADVANCED_FACE('',(#1376),#11170,.F.);
#11518=ADVANCED_FACE('',(#1377),#1049,.T.);
#11519=ADVANCED_FACE('',(#1378),#11171,.F.);
#11520=ADVANCED_FACE('',(#1379),#1050,.T.);
#11521=ADVANCED_FACE('',(#1380),#1051,.T.);
#11522=ADVANCED_FACE('',(#1381),#1052,.T.);
#11523=ADVANCED_FACE('',(#1382),#1053,.T.);
#11524=ADVANCED_FACE('',(#1383),#1054,.T.);
#11525=ADVANCED_FACE('',(#1384,#829,#830,#831,#832,#833,#834,#835,#836,
#837,#838,#839,#840,#841,#842),#1055,.T.);
#11526=ADVANCED_FACE('',(#1385),#1056,.F.);
#11527=ADVANCED_FACE('',(#1386),#1057,.T.);
#11528=ADVANCED_FACE('',(#1387),#1058,.T.);
#11529=ADVANCED_FACE('',(#1388),#1059,.T.);
#11530=ADVANCED_FACE('',(#1389),#1060,.T.);
#11531=ADVANCED_FACE('',(#1390),#1061,.T.);
#11532=ADVANCED_FACE('',(#1391),#1062,.F.);
#11533=ADVANCED_FACE('',(#1392),#1063,.T.);
#11534=ADVANCED_FACE('',(#1393),#1064,.T.);
#11535=ADVANCED_FACE('',(#1394),#1065,.T.);
#11536=ADVANCED_FACE('',(#1395),#1066,.T.);
#11537=ADVANCED_FACE('',(#1396),#1067,.T.);
#11538=ADVANCED_FACE('',(#1397),#1068,.F.);
#11539=ADVANCED_FACE('',(#1398),#11172,.F.);
#11540=ADVANCED_FACE('',(#1399),#11173,.F.);
#11541=ADVANCED_FACE('',(#1400),#11174,.F.);
#11542=ADVANCED_FACE('',(#1401),#11175,.F.);
#11543=ADVANCED_FACE('',(#1402),#11176,.F.);
#11544=ADVANCED_FACE('',(#1403),#11177,.F.);
#11545=ADVANCED_FACE('',(#1404),#11178,.F.);
#11546=ADVANCED_FACE('',(#1405),#11179,.F.);
#11547=ADVANCED_FACE('',(#1406),#11180,.F.);
#11548=ADVANCED_FACE('',(#1407,#843,#844),#1069,.T.);
#11549=ADVANCED_FACE('',(#1408,#845,#846),#1070,.T.);
#11550=ADVANCED_FACE('',(#1409),#1071,.T.);
#11551=ADVANCED_FACE('',(#1410),#1072,.T.);
#11552=ADVANCED_FACE('',(#1411,#847,#848,#849,#850,#851),#1073,.T.);
#11553=ADVANCED_FACE('',(#1412),#1074,.T.);
#11554=ADVANCED_FACE('',(#1413,#852,#853,#854,#855,#856),#1075,.T.);
#11555=ADVANCED_FACE('',(#1414),#1076,.T.);
#11556=ADVANCED_FACE('',(#1415),#1077,.T.);
#11557=ADVANCED_FACE('',(#1416,#857,#858,#859,#860),#1078,.F.);
#11558=ADVANCED_FACE('',(#1417),#11181,.F.);
#11559=ADVANCED_FACE('',(#1418),#11182,.T.);
#11560=ADVANCED_FACE('',(#1419,#861),#1079,.T.);
#11561=ADVANCED_FACE('',(#1420,#862),#1080,.F.);
#11562=ADVANCED_FACE('',(#1421),#11183,.F.);
#11563=ADVANCED_FACE('',(#1422),#11184,.F.);
#11564=ADVANCED_FACE('',(#1423),#11185,.F.);
#11565=ADVANCED_FACE('',(#1424),#11186,.F.);
#11566=ADVANCED_FACE('',(#1425,#863),#1081,.F.);
#11567=ADVANCED_FACE('',(#1426),#11187,.T.);
#11568=ADVANCED_FACE('',(#1427),#11188,.T.);
#11569=ADVANCED_FACE('',(#1428),#11189,.T.);
#11570=ADVANCED_FACE('',(#1429),#11190,.T.);
#11571=ADVANCED_FACE('',(#1430),#11191,.T.);
#11572=ADVANCED_FACE('',(#1431,#864),#1082,.T.);
#11573=ADVANCED_FACE('',(#1432),#11192,.F.);
#11574=ADVANCED_FACE('',(#1433,#865),#1083,.T.);
#11575=ADVANCED_FACE('',(#1434),#11193,.F.);
#11576=ADVANCED_FACE('',(#1435),#11194,.F.);
#11577=ADVANCED_FACE('',(#1436),#11195,.F.);
#11578=ADVANCED_FACE('',(#1437),#11196,.F.);
#11579=ADVANCED_FACE('',(#1438,#866),#1084,.F.);
#11580=ADVANCED_FACE('',(#1439),#11197,.T.);
#11581=ADVANCED_FACE('',(#1440),#11198,.T.);
#11582=ADVANCED_FACE('',(#1441),#11199,.T.);
#11583=ADVANCED_FACE('',(#1442),#11200,.T.);
#11584=ADVANCED_FACE('',(#1443),#11201,.T.);
#11585=ADVANCED_FACE('',(#1444,#867),#1085,.F.);
#11586=ADVANCED_FACE('',(#1445),#11202,.F.);
#11587=ADVANCED_FACE('',(#1446,#868),#1086,.T.);
#11588=ADVANCED_FACE('',(#1447),#11203,.F.);
#11589=ADVANCED_FACE('',(#1448,#869),#1087,.T.);
#11590=ADVANCED_FACE('',(#1449),#11204,.F.);
#11591=ADVANCED_FACE('',(#1450,#870),#1088,.T.);
#11592=ADVANCED_FACE('',(#1451),#11205,.F.);
#11593=ADVANCED_FACE('',(#1452),#11206,.F.);
#11594=ADVANCED_FACE('',(#1453),#11207,.F.);
#11595=ADVANCED_FACE('',(#1454),#1089,.T.);
#11596=ADVANCED_FACE('',(#1455,#871),#1090,.T.);
#11597=ADVANCED_FACE('',(#1456),#1091,.T.);
#11598=ADVANCED_FACE('',(#1457,#872),#1092,.T.);
#11599=ADVANCED_FACE('',(#1458,#873,#874),#1093,.T.);
#11600=ADVANCED_FACE('',(#1459,#875,#876),#1094,.F.);
#11601=ADVANCED_FACE('',(#1460),#11208,.F.);
#11602=ADVANCED_FACE('',(#1461),#11209,.T.);
#11603=ADVANCED_FACE('',(#1462,#877),#1095,.T.);
#11604=ADVANCED_FACE('',(#1463,#878),#1096,.F.);
#11605=ADVANCED_FACE('',(#1464),#11210,.F.);
#11606=ADVANCED_FACE('',(#1465,#879),#1097,.T.);
#11607=ADVANCED_FACE('',(#1466),#11211,.F.);
#11608=ADVANCED_FACE('',(#1467,#880),#1098,.T.);
#11609=ADVANCED_FACE('',(#1468),#11212,.F.);
#11610=ADVANCED_FACE('',(#1469),#11213,.F.);
#11611=ADVANCED_FACE('',(#1470),#11214,.F.);
#11612=ADVANCED_FACE('',(#1471),#1099,.T.);
#11613=ADVANCED_FACE('',(#1472,#881),#1100,.T.);
#11614=ADVANCED_FACE('',(#1473),#1101,.T.);
#11615=ADVANCED_FACE('',(#1474,#882),#1102,.T.);
#11616=ADVANCED_FACE('',(#1475,#883,#884),#1103,.T.);
#11617=ADVANCED_FACE('',(#1476,#885,#886),#1104,.F.);
#11618=ADVANCED_FACE('',(#1477),#11215,.F.);
#11619=ADVANCED_FACE('',(#1478),#11216,.T.);
#11620=ADVANCED_FACE('',(#1479,#887),#1105,.T.);
#11621=ADVANCED_FACE('',(#1480,#888),#1106,.F.);
#11622=ADVANCED_FACE('',(#1481),#11217,.F.);
#11623=ADVANCED_FACE('',(#1482),#11218,.T.);
#11624=ADVANCED_FACE('',(#1483,#889),#1107,.T.);
#11625=ADVANCED_FACE('',(#1484,#890),#1108,.F.);
#11626=ADVANCED_FACE('',(#1485),#11219,.F.);
#11627=ADVANCED_FACE('',(#1486),#11220,.F.);
#11628=ADVANCED_FACE('',(#1487),#11221,.F.);
#11629=ADVANCED_FACE('',(#1488,#891),#1109,.T.);
#11630=ADVANCED_FACE('',(#1489),#11222,.F.);
#11631=ADVANCED_FACE('',(#1490,#892),#1110,.T.);
#11632=ADVANCED_FACE('',(#1491),#1111,.T.);
#11633=ADVANCED_FACE('',(#1492),#1112,.T.);
#11634=ADVANCED_FACE('',(#1493),#1113,.T.);
#11635=ADVANCED_FACE('',(#1494),#11223,.F.);
#11636=ADVANCED_FACE('',(#1495),#11224,.F.);
#11637=ADVANCED_FACE('',(#1496),#11225,.F.);
#11638=ADVANCED_FACE('',(#1497),#1114,.T.);
#11639=ADVANCED_FACE('',(#1498),#1115,.T.);
#11640=ADVANCED_FACE('',(#1499),#1116,.T.);
#11641=ADVANCED_FACE('',(#1500),#1117,.T.);
#11642=ADVANCED_FACE('',(#1501),#1118,.T.);
#11643=ADVANCED_FACE('',(#1502,#893,#894),#1119,.F.);
#11644=ADVANCED_FACE('',(#1503),#11226,.F.);
#11645=ADVANCED_FACE('',(#1504,#895),#1120,.T.);
#11646=ADVANCED_FACE('',(#1505),#11227,.F.);
#11647=ADVANCED_FACE('',(#1506,#896),#1121,.T.);
#11648=ADVANCED_FACE('',(#1507),#11228,.F.);
#11649=ADVANCED_FACE('',(#1508,#897),#1122,.T.);
#11650=ADVANCED_FACE('',(#1509),#11229,.F.);
#11651=ADVANCED_FACE('',(#1510,#898),#1123,.T.);
#11652=ADVANCED_FACE('',(#1511),#11230,.F.);
#11653=ADVANCED_FACE('',(#1512),#11231,.F.);
#11654=ADVANCED_FACE('',(#1513),#11232,.F.);
#11655=ADVANCED_FACE('',(#1514),#11233,.F.);
#11656=ADVANCED_FACE('',(#1515),#1124,.T.);
#11657=ADVANCED_FACE('',(#1516),#1125,.T.);
#11658=ADVANCED_FACE('',(#1517),#1126,.T.);
#11659=ADVANCED_FACE('',(#1518),#1127,.T.);
#11660=ADVANCED_FACE('',(#1519,#899,#900,#901,#902),#1128,.T.);
#11661=ADVANCED_FACE('',(#1520),#1129,.T.);
#11662=ADVANCED_FACE('',(#1521),#1130,.T.);
#11663=ADVANCED_FACE('',(#1522),#1131,.T.);
#11664=ADVANCED_FACE('',(#1523),#1132,.T.);
#11665=ADVANCED_FACE('',(#1524),#1133,.T.);
#11666=ADVANCED_FACE('',(#1525,#903,#904,#905,#906),#1134,.T.);
#11667=ADVANCED_FACE('',(#1526),#1135,.T.);
#11668=ADVANCED_FACE('',(#1527),#1136,.T.);
#11669=ADVANCED_FACE('',(#1528),#1137,.F.);
#11670=ADVANCED_FACE('',(#1529),#487,.F.);
#11671=ADVANCED_FACE('',(#1530),#11234,.T.);
#11672=ADVANCED_FACE('',(#1531),#11235,.F.);
#11673=ADVANCED_FACE('',(#1532),#467,.F.);
#11674=ADVANCED_FACE('',(#1533,#907),#1138,.T.);
#11675=ADVANCED_FACE('',(#1534),#11236,.T.);
#11676=ADVANCED_FACE('',(#1535,#908),#1139,.T.);
#11677=ADVANCED_FACE('',(#1536),#468,.F.);
#11678=ADVANCED_FACE('',(#1537),#488,.F.);
#11679=ADVANCED_FACE('',(#1538),#11237,.F.);
#11680=ADVANCED_FACE('',(#1539,#909),#1140,.T.);
#11681=ADVANCED_FACE('',(#1540),#469,.T.);
#11682=ADVANCED_FACE('',(#1541),#11238,.T.);
#11683=ADVANCED_FACE('',(#1542),#470,.T.);
#11684=ADVANCED_FACE('',(#1543,#910),#1141,.T.);
#11685=ADVANCED_FACE('',(#1544),#11239,.F.);
#11686=ADVANCED_FACE('',(#1545),#437,.T.);
#11687=ADVANCED_FACE('',(#1546),#438,.T.);
#11688=ADVANCED_FACE('',(#1547),#439,.T.);
#11689=ADVANCED_FACE('',(#1548),#440,.T.);
#11690=ADVANCED_FACE('',(#1549),#441,.T.);
#11691=ADVANCED_FACE('',(#1550),#442,.T.);
#11692=ADVANCED_FACE('',(#1551),#443,.T.);
#11693=ADVANCED_FACE('',(#1552),#444,.T.);
#11694=ADVANCED_FACE('',(#1553),#445,.F.);
#11695=ADVANCED_FACE('',(#1554),#11240,.T.);
#11696=ADVANCED_FACE('',(#1555),#1142,.T.);
#11697=ADVANCED_FACE('',(#1556),#446,.F.);
#11698=ADVANCED_FACE('',(#1557),#1143,.T.);
#11699=ADVANCED_FACE('',(#1558),#447,.F.);
#11700=ADVANCED_FACE('',(#1559),#1144,.T.);
#11701=ADVANCED_FACE('',(#1560),#448,.F.);
#11702=ADVANCED_FACE('',(#1561),#1145,.T.);
#11703=ADVANCED_FACE('',(#1562),#449,.F.);
#11704=ADVANCED_FACE('',(#1563),#1146,.T.);
#11705=ADVANCED_FACE('',(#1564),#450,.F.);
#11706=ADVANCED_FACE('',(#1565),#1147,.T.);
#11707=ADVANCED_FACE('',(#1566),#451,.F.);
#11708=ADVANCED_FACE('',(#1567),#11241,.F.);
#11709=ADVANCED_FACE('',(#1568),#1148,.T.);
#11710=ADVANCED_FACE('',(#1569),#452,.F.);
#11711=ADVANCED_FACE('',(#1570,#911),#1149,.T.);
#11712=ADVANCED_FACE('',(#1571),#1150,.T.);
#11713=ADVANCED_FACE('',(#1572,#912),#1151,.T.);
#11714=ADVANCED_FACE('',(#1573),#11242,.T.);
#11715=ADVANCED_FACE('',(#1574,#913),#1152,.T.);
#11716=ADVANCED_FACE('',(#1575),#11243,.F.);
#11717=ADVANCED_FACE('',(#1576,#914),#1153,.T.);
#11718=ADVANCED_FACE('',(#1577),#11244,.T.);
#11719=ADVANCED_FACE('',(#1578,#915),#1154,.T.);
#11720=ADVANCED_FACE('',(#1579),#11245,.F.);
#11721=ADVANCED_FACE('',(#1580),#11246,.F.);
#11722=ADVANCED_FACE('',(#1581),#11247,.F.);
#11723=ADVANCED_FACE('',(#1582),#11248,.F.);
#11724=ADVANCED_FACE('',(#1583),#11249,.F.);
#11725=ADVANCED_FACE('',(#1584),#11250,.F.);
#11726=ADVANCED_FACE('',(#1585),#11251,.F.);
#11727=ADVANCED_FACE('',(#1586),#11252,.F.);
#11728=ADVANCED_FACE('',(#1587),#11253,.F.);
#11729=ADVANCED_FACE('',(#1588),#11254,.F.);
#11730=ADVANCED_FACE('',(#1589),#11255,.F.);
#11731=ADVANCED_FACE('',(#1590),#1155,.T.);
#11732=ADVANCED_FACE('',(#1591),#1156,.T.);
#11733=ADVANCED_FACE('',(#1592),#1157,.T.);
#11734=ADVANCED_FACE('',(#1593),#1158,.T.);
#11735=ADVANCED_FACE('',(#1594,#916,#917,#918,#919,#920,#921,#922,#923,
#924,#925),#1159,.T.);
#11736=ADVANCED_FACE('',(#1595,#926,#927,#928,#929,#930,#931,#932,#933,
#934,#935),#1160,.F.);
#11737=ADVANCED_FACE('',(#1596),#11256,.F.);
#11738=ADVANCED_FACE('',(#1597),#11257,.F.);
#11739=ADVANCED_FACE('',(#1598),#11258,.F.);
#11740=ADVANCED_FACE('',(#1599),#11259,.F.);
#11741=ADVANCED_FACE('',(#1600),#11260,.F.);
#11742=ADVANCED_FACE('',(#1601),#1161,.F.);
#11743=ADVANCED_FACE('',(#1602),#11261,.F.);
#11744=ADVANCED_FACE('',(#1603),#1162,.F.);
#11745=ADVANCED_FACE('',(#1604),#11262,.F.);
#11746=ADVANCED_FACE('',(#1605),#1163,.F.);
#11747=ADVANCED_FACE('',(#1606),#11263,.F.);
#11748=ADVANCED_FACE('',(#1607),#1164,.F.);
#11749=ADVANCED_FACE('',(#1608),#11264,.F.);
#11750=ADVANCED_FACE('',(#1609,#936,#937,#938,#939,#940),#1165,.T.);
#11751=ADVANCED_FACE('',(#1610,#941,#942,#943,#944,#945),#1166,.T.);
#11752=ADVANCED_FACE('',(#1611),#11265,.F.);
#11753=ADVANCED_FACE('',(#1612),#11266,.F.);
#11754=ADVANCED_FACE('',(#1613),#11267,.F.);
#11755=ADVANCED_FACE('',(#1614),#11268,.F.);
#11756=ADVANCED_FACE('',(#1615,#946,#947),#1167,.T.);
#11757=ADVANCED_FACE('',(#1616,#948,#949),#1168,.T.);
#11758=ADVANCED_FACE('',(#1617),#1169,.T.);
#11759=ADVANCED_FACE('',(#1618),#1170,.T.);
#11760=ADVANCED_FACE('',(#1619),#1171,.T.);
#11761=ADVANCED_FACE('',(#1620),#1172,.T.);
#11762=ADVANCED_FACE('',(#1621),#1173,.T.);
#11763=ADVANCED_FACE('',(#1622,#950,#951,#952,#953),#1174,.F.);
#11764=ADVANCED_FACE('',(#1623),#11269,.F.);
#11765=ADVANCED_FACE('',(#1624),#11270,.T.);
#11766=ADVANCED_FACE('',(#1625,#954),#1175,.T.);
#11767=ADVANCED_FACE('',(#1626,#955),#1176,.F.);
#11768=ADVANCED_FACE('',(#1627),#11271,.F.);
#11769=ADVANCED_FACE('',(#1628),#11272,.F.);
#11770=ADVANCED_FACE('',(#1629),#11273,.F.);
#11771=ADVANCED_FACE('',(#1630),#11274,.F.);
#11772=ADVANCED_FACE('',(#1631,#956),#1177,.F.);
#11773=ADVANCED_FACE('',(#1632),#11275,.T.);
#11774=ADVANCED_FACE('',(#1633),#11276,.T.);
#11775=ADVANCED_FACE('',(#1634),#11277,.T.);
#11776=ADVANCED_FACE('',(#1635),#11278,.T.);
#11777=ADVANCED_FACE('',(#1636),#11279,.T.);
#11778=ADVANCED_FACE('',(#1637,#957),#1178,.T.);
#11779=ADVANCED_FACE('',(#1638),#11280,.F.);
#11780=ADVANCED_FACE('',(#1639,#958),#1179,.T.);
#11781=ADVANCED_FACE('',(#1640),#11281,.F.);
#11782=ADVANCED_FACE('',(#1641),#11282,.F.);
#11783=ADVANCED_FACE('',(#1642),#11283,.F.);
#11784=ADVANCED_FACE('',(#1643),#11284,.F.);
#11785=ADVANCED_FACE('',(#1644,#959),#1180,.F.);
#11786=ADVANCED_FACE('',(#1645),#11285,.T.);
#11787=ADVANCED_FACE('',(#1646),#11286,.T.);
#11788=ADVANCED_FACE('',(#1647),#11287,.T.);
#11789=ADVANCED_FACE('',(#1648),#11288,.T.);
#11790=ADVANCED_FACE('',(#1649),#11289,.T.);
#11791=ADVANCED_FACE('',(#1650,#960),#1181,.F.);
#11792=ADVANCED_FACE('',(#1651),#11290,.F.);
#11793=ADVANCED_FACE('',(#1652,#961),#1182,.T.);
#11794=ADVANCED_FACE('',(#1653),#11291,.F.);
#11795=ADVANCED_FACE('',(#1654),#1183,.F.);
#11796=ADVANCED_FACE('',(#1655),#11292,.F.);
#11797=ADVANCED_FACE('',(#1656),#1184,.F.);
#11798=ADVANCED_FACE('',(#1657),#11293,.F.);
#11799=ADVANCED_FACE('',(#1658),#1185,.T.);
#11800=ADVANCED_FACE('',(#1659,#962),#1186,.T.);
#11801=ADVANCED_FACE('',(#1660),#1187,.T.);
#11802=ADVANCED_FACE('',(#1661,#963),#1188,.T.);
#11803=ADVANCED_FACE('',(#1662),#1189,.T.);
#11804=ADVANCED_FACE('',(#1663,#964,#965),#1190,.F.);
#11805=ADVANCED_FACE('',(#1664),#1191,.T.);
#11806=ADVANCED_FACE('',(#1665),#11294,.T.);
#11807=ADVANCED_FACE('',(#1666),#1192,.F.);
#11808=ADVANCED_FACE('',(#1667),#1193,.T.);
#11809=ADVANCED_FACE('',(#1668),#11295,.F.);
#11810=ADVANCED_FACE('',(#1669),#1194,.T.);
#11811=ADVANCED_FACE('',(#1670),#11296,.F.);
#11812=ADVANCED_FACE('',(#1671),#1195,.T.);
#11813=ADVANCED_FACE('',(#1672,#966),#1196,.T.);
#11814=ADVANCED_FACE('',(#1673),#1197,.T.);
#11815=ADVANCED_FACE('',(#1674,#967),#1198,.T.);
#11816=ADVANCED_FACE('',(#1675,#968),#1199,.T.);
#11817=ADVANCED_FACE('',(#1676),#1200,.F.);
#11818=ADVANCED_FACE('',(#1677),#1201,.T.);
#11819=ADVANCED_FACE('',(#1678),#11297,.F.);
#11820=ADVANCED_FACE('',(#1679),#1202,.T.);
#11821=ADVANCED_FACE('',(#1680),#11298,.F.);
#11822=ADVANCED_FACE('',(#1681),#1203,.T.);
#11823=ADVANCED_FACE('',(#1682),#11299,.F.);
#11824=ADVANCED_FACE('',(#1683),#1204,.T.);
#11825=ADVANCED_FACE('',(#1684),#11300,.F.);
#11826=ADVANCED_FACE('',(#1685),#1205,.T.);
#11827=ADVANCED_FACE('',(#1686),#1206,.T.);
#11828=ADVANCED_FACE('',(#1687),#1207,.T.);
#11829=ADVANCED_FACE('',(#1688),#1208,.T.);
#11830=ADVANCED_FACE('',(#1689),#1209,.T.);
#11831=ADVANCED_FACE('',(#1690,#969,#970,#971,#972),#1210,.T.);
#11832=ADVANCED_FACE('',(#1691),#1211,.T.);
#11833=ADVANCED_FACE('',(#1692),#1212,.T.);
#11834=ADVANCED_FACE('',(#1693),#1213,.T.);
#11835=ADVANCED_FACE('',(#1694),#1214,.T.);
#11836=ADVANCED_FACE('',(#1695),#1215,.T.);
#11837=ADVANCED_FACE('',(#1696),#1216,.T.);
#11838=ADVANCED_FACE('',(#1697),#1217,.T.);
#11839=ADVANCED_FACE('',(#1698),#1218,.T.);
#11840=ADVANCED_FACE('',(#1699),#1219,.T.);
#11841=ADVANCED_FACE('',(#1700),#1220,.T.);
#11842=ADVANCED_FACE('',(#1701),#1221,.T.);
#11843=ADVANCED_FACE('',(#1702),#1222,.T.);
#11844=ADVANCED_FACE('',(#1703),#1223,.T.);
#11845=ADVANCED_FACE('',(#1704),#1224,.T.);
#11846=ADVANCED_FACE('',(#1705),#1225,.T.);
#11847=ADVANCED_FACE('',(#1706),#1226,.T.);
#11848=ADVANCED_FACE('',(#1707),#1227,.T.);
#11849=ADVANCED_FACE('',(#1708),#1228,.F.);
#11850=ADVANCED_FACE('',(#1709),#1229,.T.);
#11851=ADVANCED_FACE('',(#1710),#1230,.T.);
#11852=ADVANCED_FACE('',(#1711),#1231,.T.);
#11853=ADVANCED_FACE('',(#1712),#1232,.T.);
#11854=ADVANCED_FACE('',(#1713),#1233,.T.);
#11855=ADVANCED_FACE('',(#1714),#1234,.T.);
#11856=ADVANCED_FACE('',(#1715),#1235,.T.);
#11857=ADVANCED_FACE('',(#1716),#1236,.T.);
#11858=ADVANCED_FACE('',(#1717),#1237,.T.);
#11859=ADVANCED_FACE('',(#1718),#1238,.T.);
#11860=ADVANCED_FACE('',(#1719),#1239,.F.);
#11861=ADVANCED_FACE('',(#1720),#1240,.F.);
#11862=ADVANCED_FACE('',(#1721),#1241,.F.);
#11863=ADVANCED_FACE('',(#1722),#1242,.F.);
#11864=ADVANCED_FACE('',(#1723),#1243,.F.);
#11865=ADVANCED_FACE('',(#1724),#1244,.F.);
#11866=ADVANCED_FACE('',(#1725),#1245,.F.);
#11867=ADVANCED_FACE('',(#1726),#1246,.F.);
#11868=ADVANCED_FACE('',(#1727),#1247,.F.);
#11869=ADVANCED_FACE('',(#1728),#1248,.T.);
#11870=ADVANCED_FACE('',(#1729),#471,.T.);
#11871=ADVANCED_FACE('',(#1730),#11301,.T.);
#11872=ADVANCED_FACE('',(#1731),#472,.T.);
#11873=ADVANCED_FACE('',(#1732,#973),#1249,.T.);
#11874=ADVANCED_FACE('',(#1733),#473,.T.);
#11875=ADVANCED_FACE('',(#1734),#11302,.T.);
#11876=ADVANCED_FACE('',(#1735),#489,.F.);
#11877=ADVANCED_FACE('',(#1736),#11303,.T.);
#11878=ADVANCED_FACE('',(#1737),#11304,.F.);
#11879=ADVANCED_FACE('',(#1738),#474,.F.);
#11880=ADVANCED_FACE('',(#1739,#974),#1250,.T.);
#11881=ADVANCED_FACE('',(#1740),#11305,.T.);
#11882=ADVANCED_FACE('',(#1741,#975),#1251,.T.);
#11883=ADVANCED_FACE('',(#1742),#475,.F.);
#11884=ADVANCED_FACE('',(#1743),#490,.F.);
#11885=ADVANCED_FACE('',(#1744),#11306,.F.);
#11886=ADVANCED_FACE('',(#1745,#976),#1252,.T.);
#11887=ADVANCED_FACE('',(#1746),#476,.T.);
#11888=ADVANCED_FACE('',(#1747),#11307,.T.);
#11889=ADVANCED_FACE('',(#1748),#477,.T.);
#11890=ADVANCED_FACE('',(#1749,#977),#1253,.T.);
#11891=ADVANCED_FACE('',(#1750),#11308,.F.);
#11892=ADVANCED_FACE('',(#1751),#453,.T.);
#11893=ADVANCED_FACE('',(#1752),#454,.T.);
#11894=ADVANCED_FACE('',(#1753),#455,.T.);
#11895=ADVANCED_FACE('',(#1754),#456,.T.);
#11896=ADVANCED_FACE('',(#1755),#457,.T.);
#11897=ADVANCED_FACE('',(#1756),#458,.T.);
#11898=ADVANCED_FACE('',(#1757),#459,.T.);
#11899=ADVANCED_FACE('',(#1758),#460,.F.);
#11900=ADVANCED_FACE('',(#1759),#11309,.T.);
#11901=ADVANCED_FACE('',(#1760),#1254,.T.);
#11902=ADVANCED_FACE('',(#1761),#461,.F.);
#11903=ADVANCED_FACE('',(#1762),#1255,.T.);
#11904=ADVANCED_FACE('',(#1763),#462,.F.);
#11905=ADVANCED_FACE('',(#1764),#1256,.T.);
#11906=ADVANCED_FACE('',(#1765),#463,.F.);
#11907=ADVANCED_FACE('',(#1766),#1257,.T.);
#11908=ADVANCED_FACE('',(#1767),#464,.F.);
#11909=ADVANCED_FACE('',(#1768),#1258,.T.);
#11910=ADVANCED_FACE('',(#1769),#465,.F.);
#11911=ADVANCED_FACE('',(#1770),#11310,.F.);
#11912=ADVANCED_FACE('',(#1771),#1259,.T.);
#11913=ADVANCED_FACE('',(#1772),#466,.F.);
#11914=ADVANCED_FACE('',(#1773,#978),#1260,.T.);
#11915=ADVANCED_FACE('',(#1774),#1261,.T.);
#11916=ADVANCED_FACE('',(#1775,#979),#1262,.T.);
#11917=ADVANCED_FACE('',(#1776),#11311,.T.);
#11918=ADVANCED_FACE('',(#1777,#980),#1263,.T.);
#11919=ADVANCED_FACE('',(#1778),#11312,.F.);
#11920=ADVANCED_FACE('',(#1779,#981),#1264,.T.);
#11921=ADVANCED_FACE('',(#1780),#11313,.T.);
#11922=ADVANCED_FACE('',(#1781,#982),#1265,.T.);
#11923=ADVANCED_FACE('',(#1782),#11314,.F.);
#11924=ADVANCED_FACE('',(#1783),#1266,.F.);
#11925=ADVANCED_FACE('',(#1784),#1267,.F.);
#11926=ADVANCED_FACE('',(#1785),#1268,.F.);
#11927=ADVANCED_FACE('',(#1786),#1269,.F.);
#11928=ADVANCED_FACE('',(#1787),#1270,.F.);
#11929=ADVANCED_FACE('',(#1788),#1271,.F.);
#11930=ADVANCED_FACE('',(#1789),#1272,.F.);
#11931=ADVANCED_FACE('',(#1790),#1273,.F.);
#11932=ADVANCED_FACE('',(#1791),#1274,.F.);
#11933=ADVANCED_FACE('',(#1792),#1275,.T.);
#11934=ADVANCED_FACE('',(#1793),#478,.T.);
#11935=ADVANCED_FACE('',(#1794),#11315,.T.);
#11936=ADVANCED_FACE('',(#1795),#479,.T.);
#11937=ADVANCED_FACE('',(#1796,#983),#1276,.T.);
#11938=ADVANCED_FACE('',(#1797),#480,.T.);
#11939=ADVANCED_FACE('',(#1798),#11316,.T.);
#11940=ADVANCED_FACE('',(#1799),#11317,.F.);
#11941=ADVANCED_FACE('',(#1800),#1277,.F.);
#11942=ADVANCED_FACE('',(#1801,#984),#1278,.T.);
#11943=ADVANCED_FACE('',(#1802,#985),#1279,.F.);
#11944=ADVANCED_FACE('',(#1803),#11318,.T.);
#11945=ADVANCED_FACE('',(#1804),#11319,.T.);
#11946=ADVANCED_FACE('',(#1805),#11320,.T.);
#11947=ADVANCED_FACE('',(#1806,#986),#1280,.F.);
#11948=ADVANCED_FACE('',(#1807),#11321,.T.);
#11949=ADVANCED_FACE('',(#1808),#1281,.T.);
#11950=ADVANCED_FACE('',(#1809,#987),#1282,.F.);
#11951=ADVANCED_FACE('',(#1810),#11322,.F.);
#11952=ADVANCED_FACE('',(#1811,#988),#1283,.T.);
#11953=ADVANCED_FACE('',(#1812),#11323,.F.);
#11954=ADVANCED_FACE('',(#1813),#11324,.T.);
#11955=ADVANCED_FACE('',(#1814,#989),#1284,.T.);
#11956=ADVANCED_FACE('',(#1815,#990),#1285,.F.);
#11957=ADVANCED_FACE('',(#1816),#11325,.F.);
#11958=ADVANCED_FACE('',(#1817),#11326,.T.);
#11959=ADVANCED_FACE('',(#1818,#991),#1286,.T.);
#11960=ADVANCED_FACE('',(#1819,#992),#1287,.F.);
#11961=ADVANCED_FACE('',(#1820),#11327,.T.);
#11962=ADVANCED_FACE('',(#1821),#1288,.T.);
#11963=ADVANCED_FACE('',(#1822),#1289,.F.);
#11964=ADVANCED_FACE('',(#1823),#11328,.T.);
#11965=ADVANCED_FACE('',(#1824),#1290,.T.);
#11966=ADVANCED_FACE('',(#1825),#1291,.F.);
#11967=ADVANCED_FACE('',(#1826),#11329,.F.);
#11968=ADVANCED_FACE('',(#1827),#11330,.T.);
#11969=ADVANCED_FACE('',(#1828,#993),#1292,.T.);
#11970=ADVANCED_FACE('',(#1829,#994),#1293,.F.);
#11971=ADVANCED_FACE('',(#1830),#11331,.F.);
#11972=ADVANCED_FACE('',(#1831),#11332,.F.);
#11973=ADVANCED_FACE('',(#1832,#995,#996,#997),#11333,.T.);
#11974=ADVANCED_FACE('',(#1833),#11334,.F.);
#11975=ADVANCED_FACE('',(#1834),#11335,.F.);
#11976=ADVANCED_FACE('',(#1835,#998,#999,#1000),#11336,.F.);
#11977=ADVANCED_FACE('',(#1836,#1001),#1294,.F.);
#11978=ADVANCED_FACE('',(#1837,#1002),#1295,.T.);
#11979=ADVANCED_FACE('',(#1838),#11337,.T.);
#11980=ADVANCED_FACE('',(#1839,#1003),#1296,.F.);
#11981=ADVANCED_FACE('',(#1840,#1004),#1297,.F.);
#11982=ADVANCED_FACE('',(#1841),#11338,.T.);
#11983=ADVANCED_FACE('',(#1842,#1005),#1298,.T.);
#11984=ADVANCED_FACE('',(#1843),#11339,.F.);
#11985=ADVANCED_FACE('',(#1844),#11340,.T.);
#11986=ADVANCED_FACE('',(#1845),#11341,.F.);
#11987=ADVANCED_FACE('',(#1846),#11342,.T.);
#11988=ADVANCED_FACE('',(#1847),#11343,.F.);
#11989=ADVANCED_FACE('',(#1848),#11344,.T.);
#11990=ADVANCED_FACE('',(#1849),#11345,.F.);
#11991=ADVANCED_FACE('',(#1850),#11346,.T.);
#11992=ADVANCED_FACE('',(#1851),#11347,.F.);
#11993=ADVANCED_FACE('',(#1852),#11348,.T.);
#11994=ADVANCED_FACE('',(#1853),#11349,.F.);
#11995=ADVANCED_FACE('',(#1854),#11350,.T.);
#11996=ADVANCED_FACE('',(#1855),#11351,.F.);
#11997=ADVANCED_FACE('',(#1856),#11352,.T.);
#11998=ADVANCED_FACE('',(#1857),#11353,.F.);
#11999=ADVANCED_FACE('',(#1858),#11354,.T.);
#12000=ADVANCED_FACE('',(#1859),#11355,.F.);
#12001=ADVANCED_FACE('',(#1860),#11356,.T.);
#12002=ADVANCED_FACE('',(#1861),#11357,.F.);
#12003=ADVANCED_FACE('',(#1862),#11358,.T.);
#12004=ADVANCED_FACE('',(#1863),#11359,.F.);
#12005=ADVANCED_FACE('',(#1864),#11360,.T.);
#12006=ADVANCED_FACE('',(#1865),#11361,.F.);
#12007=ADVANCED_FACE('',(#1866),#11362,.T.);
#12008=ADVANCED_FACE('',(#1867),#11363,.F.);
#12009=ADVANCED_FACE('',(#1868),#11364,.T.);
#12010=ADVANCED_FACE('',(#1869),#11365,.F.);
#12011=ADVANCED_FACE('',(#1870),#11366,.T.);
#12012=ADVANCED_FACE('',(#1871),#11367,.F.);
#12013=ADVANCED_FACE('',(#1872),#11368,.T.);
#12014=ADVANCED_FACE('',(#1873),#11369,.F.);
#12015=ADVANCED_FACE('',(#1874),#11370,.T.);
#12016=ADVANCED_FACE('',(#1875),#11371,.F.);
#12017=ADVANCED_FACE('',(#1876),#11372,.T.);
#12018=ADVANCED_FACE('',(#1877),#11373,.F.);
#12019=ADVANCED_FACE('',(#1878),#11374,.T.);
#12020=ADVANCED_FACE('',(#1879),#11375,.F.);
#12021=ADVANCED_FACE('',(#1880),#11376,.T.);
#12022=ADVANCED_FACE('',(#1881),#11377,.F.);
#12023=ADVANCED_FACE('',(#1882),#11378,.T.);
#12024=ADVANCED_FACE('',(#1883),#11379,.F.);
#12025=ADVANCED_FACE('',(#1884),#1299,.F.);
#12026=ADVANCED_FACE('',(#1885,#1006),#1300,.T.);
#12027=ADVANCED_FACE('',(#1886,#1007),#1301,.F.);
#12028=ADVANCED_FACE('',(#1887),#11380,.T.);
#12029=ADVANCED_FACE('',(#1888),#11381,.T.);
#12030=ADVANCED_FACE('',(#1889,#1008),#1302,.F.);
#12031=ADVANCED_FACE('',(#1890),#11382,.T.);
#12032=ADVANCED_FACE('',(#1891),#1303,.T.);
#12033=ADVANCED_FACE('',(#1892),#11383,.F.);
#12034=ADVANCED_FACE('',(#1893),#11384,.T.);
#12035=ADVANCED_FACE('',(#1894,#1009),#1304,.T.);
#12036=ADVANCED_FACE('',(#1895,#1010),#1305,.F.);
#12037=ADVANCED_FACE('',(#1896),#11385,.F.);
#12038=ADVANCED_FACE('',(#1897),#11386,.T.);
#12039=ADVANCED_FACE('',(#1898,#1011),#1306,.T.);
#12040=ADVANCED_FACE('',(#1899,#1012),#1307,.F.);
#12041=ADVANCED_FACE('',(#1900),#11387,.T.);
#12042=ADVANCED_FACE('',(#1901),#1308,.T.);
#12043=ADVANCED_FACE('',(#1902),#1309,.F.);
#12044=ADVANCED_FACE('',(#1903),#11388,.T.);
#12045=ADVANCED_FACE('',(#1904),#1310,.T.);
#12046=ADVANCED_FACE('',(#1905),#1311,.F.);
#12047=ADVANCED_FACE('',(#1906),#11389,.F.);
#12048=ADVANCED_FACE('',(#1907),#11390,.T.);
#12049=ADVANCED_FACE('',(#1908,#1013),#1312,.T.);
#12050=ADVANCED_FACE('',(#1909,#1014),#1313,.F.);
#12051=ADVANCED_FACE('',(#1910),#11391,.F.);
#12052=ADVANCED_FACE('',(#1911),#11392,.F.);
#12053=ADVANCED_FACE('',(#1912,#1015,#1016,#1017),#11393,.T.);
#12054=ADVANCED_FACE('',(#1913),#11394,.F.);
#12055=ADVANCED_FACE('',(#1914),#11395,.F.);
#12056=ADVANCED_FACE('',(#1915,#1018,#1019,#1020),#11396,.F.);
#12057=ADVANCED_FACE('',(#1916,#1021),#1314,.F.);
#12058=ADVANCED_FACE('',(#1917,#1022),#1315,.T.);
#12059=ADVANCED_FACE('',(#1918),#11397,.T.);
#12060=ADVANCED_FACE('',(#1919,#1023),#1316,.F.);
#12061=ADVANCED_FACE('',(#1920,#1024),#1317,.F.);
#12062=ADVANCED_FACE('',(#1921),#11398,.T.);
#12063=ADVANCED_FACE('',(#1922,#1025),#1318,.T.);
#12064=ADVANCED_FACE('',(#1923),#11399,.F.);
#12065=ADVANCED_FACE('',(#1924),#11400,.T.);
#12066=ADVANCED_FACE('',(#1925),#11401,.F.);
#12067=ADVANCED_FACE('',(#1926),#11402,.T.);
#12068=ADVANCED_FACE('',(#1927),#11403,.F.);
#12069=ADVANCED_FACE('',(#1928),#11404,.T.);
#12070=ADVANCED_FACE('',(#1929),#11405,.F.);
#12071=ADVANCED_FACE('',(#1930),#11406,.T.);
#12072=ADVANCED_FACE('',(#1931),#11407,.F.);
#12073=ADVANCED_FACE('',(#1932),#11408,.T.);
#12074=ADVANCED_FACE('',(#1933),#11409,.F.);
#12075=ADVANCED_FACE('',(#1934),#11410,.T.);
#12076=ADVANCED_FACE('',(#1935),#11411,.F.);
#12077=ADVANCED_FACE('',(#1936),#11412,.T.);
#12078=ADVANCED_FACE('',(#1937),#11413,.F.);
#12079=ADVANCED_FACE('',(#1938),#11414,.T.);
#12080=ADVANCED_FACE('',(#1939),#11415,.F.);
#12081=ADVANCED_FACE('',(#1940),#11416,.T.);
#12082=ADVANCED_FACE('',(#1941),#11417,.F.);
#12083=ADVANCED_FACE('',(#1942),#11418,.T.);
#12084=ADVANCED_FACE('',(#1943),#11419,.F.);
#12085=ADVANCED_FACE('',(#1944),#11420,.T.);
#12086=ADVANCED_FACE('',(#1945),#11421,.F.);
#12087=ADVANCED_FACE('',(#1946),#11422,.T.);
#12088=ADVANCED_FACE('',(#1947),#11423,.F.);
#12089=ADVANCED_FACE('',(#1948),#11424,.T.);
#12090=ADVANCED_FACE('',(#1949),#11425,.F.);
#12091=ADVANCED_FACE('',(#1950),#11426,.T.);
#12092=ADVANCED_FACE('',(#1951),#11427,.F.);
#12093=ADVANCED_FACE('',(#1952),#11428,.T.);
#12094=ADVANCED_FACE('',(#1953),#11429,.F.);
#12095=ADVANCED_FACE('',(#1954),#11430,.T.);
#12096=ADVANCED_FACE('',(#1955),#11431,.F.);
#12097=ADVANCED_FACE('',(#1956),#11432,.T.);
#12098=ADVANCED_FACE('',(#1957),#11433,.F.);
#12099=ADVANCED_FACE('',(#1958),#11434,.T.);
#12100=ADVANCED_FACE('',(#1959),#11435,.F.);
#12101=ADVANCED_FACE('',(#1960),#11436,.T.);
#12102=ADVANCED_FACE('',(#1961),#11437,.F.);
#12103=ADVANCED_FACE('',(#1962),#11438,.T.);
#12104=ADVANCED_FACE('',(#1963),#11439,.F.);
#12105=ADVANCED_FACE('',(#1964),#11440,.T.);
#12106=ADVANCED_FACE('',(#1965),#11441,.F.);
#12107=ADVANCED_FACE('',(#1966),#11442,.T.);
#12108=ADVANCED_FACE('',(#1967),#11443,.F.);
#12109=ADVANCED_FACE('',(#1968),#11444,.T.);
#12110=ADVANCED_FACE('',(#1969),#11445,.F.);
#12111=ADVANCED_FACE('',(#1970),#11446,.T.);
#12112=ADVANCED_FACE('',(#1971),#11447,.F.);
#12113=ADVANCED_FACE('',(#1972),#11448,.T.);
#12114=ADVANCED_FACE('',(#1973),#11449,.F.);
#12115=ADVANCED_FACE('',(#1974),#11450,.T.);
#12116=ADVANCED_FACE('',(#1975),#11451,.F.);
#12117=ADVANCED_FACE('',(#1976),#11452,.T.);
#12118=ADVANCED_FACE('',(#1977),#11453,.F.);
#12119=ADVANCED_FACE('',(#1978),#11454,.T.);
#12120=ADVANCED_FACE('',(#1979),#11455,.F.);
#12121=ADVANCED_FACE('',(#1980),#11456,.T.);
#12122=ADVANCED_FACE('',(#1981),#11457,.F.);
#12123=ADVANCED_FACE('',(#1982),#11458,.T.);
#12124=ADVANCED_FACE('',(#1983),#11459,.F.);
#12125=ADVANCED_FACE('',(#1984),#11460,.T.);
#12126=ADVANCED_FACE('',(#1985),#11461,.F.);
#12127=ADVANCED_FACE('',(#1986),#11462,.T.);
#12128=ADVANCED_FACE('',(#1987),#11463,.F.);
#12129=ADVANCED_FACE('',(#1988),#11464,.T.);
#12130=ADVANCED_FACE('',(#1989),#11465,.F.);
#12131=ADVANCED_FACE('',(#1990),#11466,.T.);
#12132=ADVANCED_FACE('',(#1991),#11467,.F.);
#12133=ADVANCED_FACE('',(#1992),#11468,.T.);
#12134=ADVANCED_FACE('',(#1993),#11469,.F.);
#12135=ADVANCED_FACE('',(#1994),#11470,.T.);
#12136=ADVANCED_FACE('',(#1995),#11471,.F.);
#12137=ADVANCED_FACE('',(#1996),#11472,.T.);
#12138=ADVANCED_FACE('',(#1997),#11473,.F.);
#12139=ADVANCED_FACE('',(#1998),#11474,.T.);
#12140=ADVANCED_FACE('',(#1999),#11475,.F.);
#12141=ADVANCED_FACE('',(#2000),#11476,.T.);
#12142=ADVANCED_FACE('',(#2001),#11477,.F.);
#12143=ADVANCED_FACE('',(#2002),#11478,.T.);
#12144=ADVANCED_FACE('',(#2003),#1319,.T.);
#12145=ADVANCED_FACE('',(#2004),#481,.T.);
#12146=ADVANCED_FACE('',(#2005),#11479,.T.);
#12147=ADVANCED_FACE('',(#2006),#482,.T.);
#12148=ADVANCED_FACE('',(#2007,#1026),#1320,.T.);
#12149=ADVANCED_FACE('',(#2008),#483,.T.);
#12150=ADVANCED_FACE('',(#2009),#11480,.T.);
#12151=ADVANCED_FACE('',(#2010),#484,.T.);
#12152=ADVANCED_FACE('',(#2011),#1321,.T.);
#12153=ADVANCED_FACE('',(#2012),#1322,.F.);
#12154=ADVANCED_FACE('',(#2013),#1323,.F.);
#12155=ADVANCED_FACE('',(#2014),#1324,.F.);
#12156=ADVANCED_FACE('',(#2015),#1325,.F.);
#12157=ADVANCED_FACE('',(#2016),#1326,.F.);
#12158=ADVANCED_FACE('',(#2017),#1327,.F.);
#12159=ADVANCED_FACE('',(#2018),#1328,.F.);
#12160=ADVANCED_FACE('',(#2019),#1329,.F.);
#12161=ADVANCED_FACE('',(#2020),#11481,.T.);
#12162=ADVANCED_FACE('',(#2021),#1330,.F.);
#12163=ADVANCED_FACE('',(#2022,#1027),#1331,.T.);
#12164=ADVANCED_FACE('',(#2023,#1028),#1332,.F.);
#12165=ADVANCED_FACE('',(#2024),#11482,.T.);
#12166=ADVANCED_FACE('',(#2025),#11483,.T.);
#12167=ADVANCED_FACE('',(#2026,#1029),#1333,.T.);
#12168=ADVANCED_FACE('',(#2027,#1030),#1334,.F.);
#12169=ADVANCED_FACE('',(#2028),#11484,.T.);
#12170=ADVANCED_FACE('',(#2029),#11485,.T.);
#12171=ADVANCED_FACE('',(#2030,#1031),#1335,.F.);
#12172=ADVANCED_FACE('',(#2031),#11486,.T.);
#12173=ADVANCED_FACE('',(#2032,#1032),#1336,.T.);
#12174=ADVANCED_FACE('',(#2033),#11487,.T.);
#12175=ADVANCED_FACE('',(#2034),#11488,.T.);
#12176=ADVANCED_FACE('',(#2035),#1337,.T.);
#12177=ADVANCED_FACE('',(#2036,#1033),#1338,.F.);
#12178=ADVANCED_FACE('',(#2037),#1339,.T.);
#12179=ADVANCED_FACE('',(#2038),#11489,.F.);
#12180=ADVANCED_FACE('',(#2039),#1340,.T.);
#12181=ADVANCED_FACE('',(#2040),#11490,.F.);
#12182=ADVANCED_FACE('',(#2041),#11491,.T.);
#12183=ADVANCED_FACE('',(#2042,#1034),#1341,.T.);
#12184=ADVANCED_FACE('',(#2043,#1035),#1342,.F.);
#12185=ADVANCED_FACE('',(#2044),#1343,.F.);
#12186=ADVANCED_FACE('',(#2045),#1344,.F.);
#12187=ADVANCED_FACE('',(#2046),#1345,.F.);
#12188=ADVANCED_FACE('',(#2047),#1346,.F.);
#12189=ADVANCED_FACE('',(#2048),#1347,.F.);
#12190=ADVANCED_FACE('',(#2049),#1348,.F.);
#12191=ADVANCED_FACE('',(#2050),#1349,.F.);
#12192=ADVANCED_FACE('',(#2051,#1036),#1350,.T.);
#12193=ADVANCED_FACE('',(#2052),#485,.T.);
#12194=ADVANCED_FACE('',(#2053),#11492,.T.);
#12195=ADVANCED_FACE('',(#2054),#486,.T.);
#12196=ADVANCED_FACE('',(#2055),#1351,.T.);
#12197=CLOSED_SHELL('',(#11493,#11494,#11495,#11496,#11497,#11498,#11499,
#11500,#11501,#11502,#11503,#11504,#11505,#11506,#11507,#11508,#11509,#11510,
#11511,#11512,#11513,#11514,#11515,#11516,#11517,#11518,#11519,#11520,#11521,
#11522,#11523,#11524,#11525,#11526));
#12198=CLOSED_SHELL('',(#11527,#11528,#11529,#11530,#11531,#11532));
#12199=CLOSED_SHELL('',(#11533,#11534,#11535,#11536,#11537,#11538));
#12200=CLOSED_SHELL('',(#11539,#11540,#11541,#11542,#11543,#11544,#11545,
#11546,#11547,#11548,#11549,#11550,#11551,#11552,#11553,#11554,#11555,#11556,
#11557));
#12201=CLOSED_SHELL('',(#11558,#11559,#11560,#11561));
#12202=CLOSED_SHELL('',(#11562,#11563,#11564,#11565,#11566,#11567,#11568,
#11569,#11570,#11571,#11572,#11573,#11574));
#12203=CLOSED_SHELL('',(#11575,#11576,#11577,#11578,#11579,#11580,#11581,
#11582,#11583,#11584,#11585,#11586,#11587));
#12204=CLOSED_SHELL('',(#11588,#11589,#11590,#11591,#11592,#11593,#11594,
#11595,#11596,#11597,#11598,#11599,#11600));
#12205=CLOSED_SHELL('',(#11601,#11602,#11603,#11604));
#12206=CLOSED_SHELL('',(#11605,#11606,#11607,#11608,#11609,#11610,#11611,
#11612,#11613,#11614,#11615,#11616,#11617));
#12207=CLOSED_SHELL('',(#11618,#11619,#11620,#11621));
#12208=CLOSED_SHELL('',(#11622,#11623,#11624,#11625));
#12209=CLOSED_SHELL('',(#11626,#11627,#11628,#11629,#11630,#11631,#11632,
#11633,#11634,#11635,#11636,#11637,#11638,#11639,#11640,#11641,#11642,#11643));
#12210=CLOSED_SHELL('',(#11644,#11645,#11646,#11647,#11648,#11649,#11650,
#11651,#11652,#11653,#11654,#11655,#11656,#11657,#11658,#11659,#11660,#11661,
#11662,#11663,#11664,#11665,#11666,#11667,#11668,#11669));
#12211=CLOSED_SHELL('',(#11670,#11671,#11672,#11673,#11674,#11675,#11676,
#11677));
#12212=CLOSED_SHELL('',(#11678,#11679,#11680,#11681,#11682,#11683,#11684,
#11685));
#12213=CLOSED_SHELL('',(#11686));
#12214=CLOSED_SHELL('',(#11687));
#12215=CLOSED_SHELL('',(#11688));
#12216=CLOSED_SHELL('',(#11689));
#12217=CLOSED_SHELL('',(#11690));
#12218=CLOSED_SHELL('',(#11691));
#12219=CLOSED_SHELL('',(#11692));
#12220=CLOSED_SHELL('',(#11693));
#12221=CLOSED_SHELL('',(#11694,#11695,#11696,#11697,#11698,#11699,#11700,
#11701,#11702,#11703,#11704,#11705,#11706,#11707,#11708,#11709,#11710,#11711,
#11712));
#12222=CLOSED_SHELL('',(#11713,#11714,#11715,#11716));
#12223=CLOSED_SHELL('',(#11717,#11718,#11719,#11720));
#12224=CLOSED_SHELL('',(#11721,#11722,#11723,#11724,#11725,#11726,#11727,
#11728,#11729,#11730,#11731,#11732,#11733,#11734,#11735,#11736));
#12225=CLOSED_SHELL('',(#11737,#11738,#11739,#11740,#11741,#11742,#11743,
#11744,#11745,#11746,#11747,#11748,#11749,#11750,#11751,#11752,#11753,#11754,
#11755,#11756,#11757,#11758,#11759,#11760,#11761,#11762,#11763));
#12226=CLOSED_SHELL('',(#11764,#11765,#11766,#11767));
#12227=CLOSED_SHELL('',(#11768,#11769,#11770,#11771,#11772,#11773,#11774,
#11775,#11776,#11777,#11778,#11779,#11780));
#12228=CLOSED_SHELL('',(#11781,#11782,#11783,#11784,#11785,#11786,#11787,
#11788,#11789,#11790,#11791,#11792,#11793));
#12229=CLOSED_SHELL('',(#11794,#11795,#11796,#11797,#11798,#11799,#11800,
#11801,#11802,#11803,#11804));
#12230=CLOSED_SHELL('',(#11805,#11806,#11807));
#12231=CLOSED_SHELL('',(#11808,#11809,#11810,#11811,#11812,#11813,#11814,
#11815,#11816,#11817));
#12232=CLOSED_SHELL('',(#11818,#11819,#11820,#11821,#11822,#11823,#11824,
#11825,#11826,#11827,#11828,#11829,#11830,#11831,#11832,#11833,#11834,#11835,
#11836,#11837,#11838,#11839));
#12233=CLOSED_SHELL('',(#11840,#11841,#11842,#11843,#11844,#11845,#11846,
#11847,#11848,#11849));
#12234=CLOSED_SHELL('',(#11850,#11851,#11852,#11853,#11854,#11855,#11856,
#11857,#11858,#11859));
#12235=CLOSED_SHELL('',(#11860,#11861,#11862,#11863,#11864,#11865,#11866,
#11867));
#12236=CLOSED_SHELL('',(#11868,#11869,#11870,#11871,#11872,#11873,#11874,
#11875));
#12237=CLOSED_SHELL('',(#11876,#11877,#11878,#11879,#11880,#11881,#11882,
#11883));
#12238=CLOSED_SHELL('',(#11884,#11885,#11886,#11887,#11888,#11889,#11890,
#11891));
#12239=CLOSED_SHELL('',(#11892));
#12240=CLOSED_SHELL('',(#11893));
#12241=CLOSED_SHELL('',(#11894));
#12242=CLOSED_SHELL('',(#11895));
#12243=CLOSED_SHELL('',(#11896));
#12244=CLOSED_SHELL('',(#11897));
#12245=CLOSED_SHELL('',(#11898));
#12246=CLOSED_SHELL('',(#11899,#11900,#11901,#11902,#11903,#11904,#11905,
#11906,#11907,#11908,#11909,#11910,#11911,#11912,#11913,#11914,#11915));
#12247=CLOSED_SHELL('',(#11916,#11917,#11918,#11919));
#12248=CLOSED_SHELL('',(#11920,#11921,#11922,#11923));
#12249=CLOSED_SHELL('',(#11924,#11925,#11926,#11927,#11928,#11929,#11930,
#11931));
#12250=CLOSED_SHELL('',(#11932,#11933,#11934,#11935,#11936,#11937,#11938,
#11939));
#12251=CLOSED_SHELL('',(#11940,#11941,#11942,#11943,#11944,#11945,#11946,
#11947,#11948,#11949,#11950));
#12252=CLOSED_SHELL('',(#11951,#11952,#11953,#11954,#11955,#11956));
#12253=CLOSED_SHELL('',(#11957,#11958,#11959,#11960));
#12254=CLOSED_SHELL('',(#11961,#11962,#11963));
#12255=CLOSED_SHELL('',(#11964,#11965,#11966));
#12256=CLOSED_SHELL('',(#11967,#11968,#11969,#11970));
#12257=CLOSED_SHELL('',(#11971,#11972,#11973,#11974,#11975,#11976,#11977,
#11978,#11979,#11980,#11981,#11982,#11983,#11984,#11985,#11986,#11987,#11988,
#11989,#11990,#11991,#11992,#11993,#11994,#11995,#11996,#11997,#11998,#11999,
#12000,#12001,#12002,#12003,#12004,#12005,#12006,#12007,#12008,#12009,#12010,
#12011,#12012,#12013,#12014,#12015,#12016,#12017,#12018,#12019,#12020,#12021,
#12022,#12023));
#12258=CLOSED_SHELL('',(#12024,#12025,#12026,#12027,#12028,#12029,#12030,
#12031,#12032));
#12259=CLOSED_SHELL('',(#12033,#12034,#12035,#12036));
#12260=CLOSED_SHELL('',(#12037,#12038,#12039,#12040));
#12261=CLOSED_SHELL('',(#12041,#12042,#12043));
#12262=CLOSED_SHELL('',(#12044,#12045,#12046));
#12263=CLOSED_SHELL('',(#12047,#12048,#12049,#12050));
#12264=CLOSED_SHELL('',(#12051,#12052,#12053,#12054,#12055,#12056,#12057,
#12058,#12059,#12060,#12061,#12062,#12063,#12064,#12065,#12066,#12067,#12068,
#12069,#12070,#12071,#12072,#12073,#12074,#12075,#12076,#12077,#12078,#12079,
#12080,#12081,#12082,#12083,#12084,#12085,#12086,#12087,#12088,#12089,#12090,
#12091,#12092,#12093,#12094,#12095,#12096,#12097,#12098,#12099,#12100,#12101,
#12102,#12103,#12104,#12105,#12106,#12107,#12108,#12109,#12110,#12111,#12112,
#12113,#12114,#12115,#12116,#12117,#12118,#12119,#12120,#12121,#12122,#12123,
#12124,#12125,#12126,#12127,#12128,#12129,#12130,#12131,#12132,#12133,#12134,
#12135,#12136,#12137,#12138,#12139,#12140,#12141,#12142,#12143));
#12265=CLOSED_SHELL('',(#12144,#12145,#12146,#12147,#12148,#12149,#12150,
#12151,#12152));
#12266=CLOSED_SHELL('',(#12153,#12154,#12155,#12156,#12157,#12158,#12159,
#12160));
#12267=CLOSED_SHELL('',(#12161,#12162,#12163,#12164,#12165,#12166,#12167,
#12168,#12169,#12170,#12171,#12172,#12173,#12174,#12175,#12176,#12177));
#12268=CLOSED_SHELL('',(#12178,#12179,#12180,#12181,#12182,#12183,#12184));
#12269=CLOSED_SHELL('',(#12185,#12186,#12187,#12188,#12189,#12190,#12191,
#12192,#12193,#12194,#12195,#12196));
#12270=DERIVED_UNIT_ELEMENT(#12380,1.);
#12271=DERIVED_UNIT_ELEMENT(#23589,-3.);
#12272=DERIVED_UNIT_ELEMENT(#12380,1.);
#12273=DERIVED_UNIT_ELEMENT(#23589,-3.);
#12274=DERIVED_UNIT_ELEMENT(#12380,1.);
#12275=DERIVED_UNIT_ELEMENT(#23589,-3.);
#12276=DERIVED_UNIT_ELEMENT(#12380,1.);
#12277=DERIVED_UNIT_ELEMENT(#23589,-3.);
#12278=DERIVED_UNIT_ELEMENT(#12380,1.);
#12279=DERIVED_UNIT_ELEMENT(#23589,-3.);
#12280=DERIVED_UNIT_ELEMENT(#12380,1.);
#12281=DERIVED_UNIT_ELEMENT(#23589,-3.);
#12282=DERIVED_UNIT_ELEMENT(#12380,1.);
#12283=DERIVED_UNIT_ELEMENT(#23589,-3.);
#12284=DERIVED_UNIT_ELEMENT(#12380,1.);
#12285=DERIVED_UNIT_ELEMENT(#23589,-3.);
#12286=DERIVED_UNIT_ELEMENT(#12380,1.);
#12287=DERIVED_UNIT_ELEMENT(#23589,-3.);
#12288=DERIVED_UNIT_ELEMENT(#12380,1.);
#12289=DERIVED_UNIT_ELEMENT(#23589,-3.);
#12290=DERIVED_UNIT_ELEMENT(#12380,1.);
#12291=DERIVED_UNIT_ELEMENT(#23589,-3.);
#12292=DERIVED_UNIT_ELEMENT(#12380,1.);
#12293=DERIVED_UNIT_ELEMENT(#23589,-3.);
#12294=DERIVED_UNIT_ELEMENT(#12380,1.);
#12295=DERIVED_UNIT_ELEMENT(#23589,-3.);
#12296=DERIVED_UNIT_ELEMENT(#12380,1.);
#12297=DERIVED_UNIT_ELEMENT(#23589,-3.);
#12298=DERIVED_UNIT_ELEMENT(#12380,1.);
#12299=DERIVED_UNIT_ELEMENT(#23589,-3.);
#12300=DERIVED_UNIT_ELEMENT(#12380,1.);
#12301=DERIVED_UNIT_ELEMENT(#23589,-3.);
#12302=DERIVED_UNIT_ELEMENT(#12380,1.);
#12303=DERIVED_UNIT_ELEMENT(#23589,-3.);
#12304=DERIVED_UNIT_ELEMENT(#12380,1.);
#12305=DERIVED_UNIT_ELEMENT(#23589,-3.);
#12306=DERIVED_UNIT_ELEMENT(#12380,1.);
#12307=DERIVED_UNIT_ELEMENT(#23589,-3.);
#12308=DERIVED_UNIT_ELEMENT(#12380,1.);
#12309=DERIVED_UNIT_ELEMENT(#23589,-3.);
#12310=DERIVED_UNIT_ELEMENT(#12380,1.);
#12311=DERIVED_UNIT_ELEMENT(#23589,-3.);
#12312=DERIVED_UNIT_ELEMENT(#12380,1.);
#12313=DERIVED_UNIT_ELEMENT(#23589,-3.);
#12314=DERIVED_UNIT_ELEMENT(#12380,1.);
#12315=DERIVED_UNIT_ELEMENT(#23589,-3.);
#12316=DERIVED_UNIT_ELEMENT(#12380,1.);
#12317=DERIVED_UNIT_ELEMENT(#23589,-3.);
#12318=DERIVED_UNIT_ELEMENT(#12380,1.);
#12319=DERIVED_UNIT_ELEMENT(#23589,-3.);
#12320=DERIVED_UNIT_ELEMENT(#12380,1.);
#12321=DERIVED_UNIT_ELEMENT(#23589,-3.);
#12322=DERIVED_UNIT_ELEMENT(#12380,1.);
#12323=DERIVED_UNIT_ELEMENT(#23589,-3.);
#12324=DERIVED_UNIT_ELEMENT(#12380,1.);
#12325=DERIVED_UNIT_ELEMENT(#23589,-3.);
#12326=DERIVED_UNIT_ELEMENT(#12380,1.);
#12327=DERIVED_UNIT_ELEMENT(#23589,-3.);
#12328=DERIVED_UNIT_ELEMENT(#12380,1.);
#12329=DERIVED_UNIT_ELEMENT(#23589,-3.);
#12330=DERIVED_UNIT_ELEMENT(#12380,1.);
#12331=DERIVED_UNIT_ELEMENT(#23589,-3.);
#12332=DERIVED_UNIT_ELEMENT(#12380,1.);
#12333=DERIVED_UNIT_ELEMENT(#23589,-3.);
#12334=DERIVED_UNIT_ELEMENT(#12380,1.);
#12335=DERIVED_UNIT_ELEMENT(#23589,-3.);
#12336=DERIVED_UNIT_ELEMENT(#12380,1.);
#12337=DERIVED_UNIT_ELEMENT(#23589,-3.);
#12338=DERIVED_UNIT_ELEMENT(#12380,1.);
#12339=DERIVED_UNIT_ELEMENT(#23589,-3.);
#12340=DERIVED_UNIT_ELEMENT(#12380,1.);
#12341=DERIVED_UNIT_ELEMENT(#23589,-3.);
#12342=DERIVED_UNIT_ELEMENT(#12380,1.);
#12343=DERIVED_UNIT_ELEMENT(#23589,-3.);
#12344=DERIVED_UNIT_ELEMENT(#12380,1.);
#12345=DERIVED_UNIT_ELEMENT(#23589,-3.);
#12346=DERIVED_UNIT_ELEMENT(#12380,1.);
#12347=DERIVED_UNIT_ELEMENT(#23589,-3.);
#12348=DERIVED_UNIT_ELEMENT(#12380,1.);
#12349=DERIVED_UNIT_ELEMENT(#23589,-3.);
#12350=DERIVED_UNIT_ELEMENT(#12380,1.);
#12351=DERIVED_UNIT_ELEMENT(#23589,-3.);
#12352=DERIVED_UNIT_ELEMENT(#12380,1.);
#12353=DERIVED_UNIT_ELEMENT(#23589,-3.);
#12354=DERIVED_UNIT_ELEMENT(#12380,1.);
#12355=DERIVED_UNIT_ELEMENT(#23589,-3.);
#12356=DERIVED_UNIT_ELEMENT(#12380,1.);
#12357=DERIVED_UNIT_ELEMENT(#23589,-3.);
#12358=DERIVED_UNIT_ELEMENT(#12380,1.);
#12359=DERIVED_UNIT_ELEMENT(#23589,-3.);
#12360=DERIVED_UNIT_ELEMENT(#12380,1.);
#12361=DERIVED_UNIT_ELEMENT(#23589,-3.);
#12362=DERIVED_UNIT_ELEMENT(#12380,1.);
#12363=DERIVED_UNIT_ELEMENT(#23589,-3.);
#12364=DERIVED_UNIT_ELEMENT(#12380,1.);
#12365=DERIVED_UNIT_ELEMENT(#23589,-3.);
#12366=DERIVED_UNIT_ELEMENT(#12380,1.);
#12367=DERIVED_UNIT_ELEMENT(#23589,-3.);
#12368=DERIVED_UNIT_ELEMENT(#12380,1.);
#12369=DERIVED_UNIT_ELEMENT(#23589,-3.);
#12370=DERIVED_UNIT_ELEMENT(#12380,1.);
#12371=DERIVED_UNIT_ELEMENT(#23589,-3.);
#12372=DERIVED_UNIT_ELEMENT(#12380,1.);
#12373=DERIVED_UNIT_ELEMENT(#23589,-3.);
#12374=DERIVED_UNIT_ELEMENT(#12380,1.);
#12375=DERIVED_UNIT_ELEMENT(#23589,-3.);
#12376=DERIVED_UNIT_ELEMENT(#12380,1.);
#12377=DERIVED_UNIT_ELEMENT(#23589,-3.);
#12378=DERIVED_UNIT_ELEMENT(#12380,1.);
#12379=DERIVED_UNIT_ELEMENT(#23589,-3.);
#12380=(
MASS_UNIT()
NAMED_UNIT(*)
SI_UNIT(.KILO.,.GRAM.)
);
#12381=DERIVED_UNIT((#12270,#12271));
#12382=DERIVED_UNIT((#12272,#12273));
#12383=DERIVED_UNIT((#12274,#12275));
#12384=DERIVED_UNIT((#12276,#12277));
#12385=DERIVED_UNIT((#12278,#12279));
#12386=DERIVED_UNIT((#12280,#12281));
#12387=DERIVED_UNIT((#12282,#12283));
#12388=DERIVED_UNIT((#12284,#12285));
#12389=DERIVED_UNIT((#12286,#12287));
#12390=DERIVED_UNIT((#12288,#12289));
#12391=DERIVED_UNIT((#12290,#12291));
#12392=DERIVED_UNIT((#12292,#12293));
#12393=DERIVED_UNIT((#12294,#12295));
#12394=DERIVED_UNIT((#12296,#12297));
#12395=DERIVED_UNIT((#12298,#12299));
#12396=DERIVED_UNIT((#12300,#12301));
#12397=DERIVED_UNIT((#12302,#12303));
#12398=DERIVED_UNIT((#12304,#12305));
#12399=DERIVED_UNIT((#12306,#12307));
#12400=DERIVED_UNIT((#12308,#12309));
#12401=DERIVED_UNIT((#12310,#12311));
#12402=DERIVED_UNIT((#12312,#12313));
#12403=DERIVED_UNIT((#12314,#12315));
#12404=DERIVED_UNIT((#12316,#12317));
#12405=DERIVED_UNIT((#12318,#12319));
#12406=DERIVED_UNIT((#12320,#12321));
#12407=DERIVED_UNIT((#12322,#12323));
#12408=DERIVED_UNIT((#12324,#12325));
#12409=DERIVED_UNIT((#12326,#12327));
#12410=DERIVED_UNIT((#12328,#12329));
#12411=DERIVED_UNIT((#12330,#12331));
#12412=DERIVED_UNIT((#12332,#12333));
#12413=DERIVED_UNIT((#12334,#12335));
#12414=DERIVED_UNIT((#12336,#12337));
#12415=DERIVED_UNIT((#12338,#12339));
#12416=DERIVED_UNIT((#12340,#12341));
#12417=DERIVED_UNIT((#12342,#12343));
#12418=DERIVED_UNIT((#12344,#12345));
#12419=DERIVED_UNIT((#12346,#12347));
#12420=DERIVED_UNIT((#12348,#12349));
#12421=DERIVED_UNIT((#12350,#12351));
#12422=DERIVED_UNIT((#12352,#12353));
#12423=DERIVED_UNIT((#12354,#12355));
#12424=DERIVED_UNIT((#12356,#12357));
#12425=DERIVED_UNIT((#12358,#12359));
#12426=DERIVED_UNIT((#12360,#12361));
#12427=DERIVED_UNIT((#12362,#12363));
#12428=DERIVED_UNIT((#12364,#12365));
#12429=DERIVED_UNIT((#12366,#12367));
#12430=DERIVED_UNIT((#12368,#12369));
#12431=DERIVED_UNIT((#12370,#12371));
#12432=DERIVED_UNIT((#12372,#12373));
#12433=DERIVED_UNIT((#12374,#12375));
#12434=DERIVED_UNIT((#12376,#12377));
#12435=DERIVED_UNIT((#12378,#12379));
#12436=MEASURE_REPRESENTATION_ITEM('density measure',
POSITIVE_RATIO_MEASURE(7850.),#12381);
#12437=MEASURE_REPRESENTATION_ITEM('density measure',
POSITIVE_RATIO_MEASURE(7850.),#12382);
#12438=MEASURE_REPRESENTATION_ITEM('density measure',
POSITIVE_RATIO_MEASURE(7850.),#12383);
#12439=MEASURE_REPRESENTATION_ITEM('density measure',
POSITIVE_RATIO_MEASURE(7850.),#12384);
#12440=MEASURE_REPRESENTATION_ITEM('density measure',
POSITIVE_RATIO_MEASURE(7850.),#12385);
#12441=MEASURE_REPRESENTATION_ITEM('density measure',
POSITIVE_RATIO_MEASURE(7850.),#12386);
#12442=MEASURE_REPRESENTATION_ITEM('density measure',
POSITIVE_RATIO_MEASURE(7850.),#12387);
#12443=MEASURE_REPRESENTATION_ITEM('density measure',
POSITIVE_RATIO_MEASURE(7850.),#12388);
#12444=MEASURE_REPRESENTATION_ITEM('density measure',
POSITIVE_RATIO_MEASURE(7850.),#12389);
#12445=MEASURE_REPRESENTATION_ITEM('density measure',
POSITIVE_RATIO_MEASURE(7850.),#12390);
#12446=MEASURE_REPRESENTATION_ITEM('density measure',
POSITIVE_RATIO_MEASURE(7850.),#12391);
#12447=MEASURE_REPRESENTATION_ITEM('density measure',
POSITIVE_RATIO_MEASURE(7850.),#12392);
#12448=MEASURE_REPRESENTATION_ITEM('density measure',
POSITIVE_RATIO_MEASURE(7850.),#12393);
#12449=MEASURE_REPRESENTATION_ITEM('density measure',
POSITIVE_RATIO_MEASURE(7850.),#12394);
#12450=MEASURE_REPRESENTATION_ITEM('density measure',
POSITIVE_RATIO_MEASURE(7850.),#12395);
#12451=MEASURE_REPRESENTATION_ITEM('density measure',
POSITIVE_RATIO_MEASURE(7850.),#12396);
#12452=MEASURE_REPRESENTATION_ITEM('density measure',
POSITIVE_RATIO_MEASURE(7850.),#12397);
#12453=MEASURE_REPRESENTATION_ITEM('density measure',
POSITIVE_RATIO_MEASURE(7850.),#12398);
#12454=MEASURE_REPRESENTATION_ITEM('density measure',
POSITIVE_RATIO_MEASURE(7850.),#12399);
#12455=MEASURE_REPRESENTATION_ITEM('density measure',
POSITIVE_RATIO_MEASURE(7850.),#12400);
#12456=MEASURE_REPRESENTATION_ITEM('density measure',
POSITIVE_RATIO_MEASURE(7850.),#12401);
#12457=MEASURE_REPRESENTATION_ITEM('density measure',
POSITIVE_RATIO_MEASURE(7850.),#12402);
#12458=MEASURE_REPRESENTATION_ITEM('density measure',
POSITIVE_RATIO_MEASURE(7850.),#12403);
#12459=MEASURE_REPRESENTATION_ITEM('density measure',
POSITIVE_RATIO_MEASURE(7850.),#12404);
#12460=MEASURE_REPRESENTATION_ITEM('density measure',
POSITIVE_RATIO_MEASURE(7850.),#12405);
#12461=MEASURE_REPRESENTATION_ITEM('density measure',
POSITIVE_RATIO_MEASURE(7850.),#12406);
#12462=MEASURE_REPRESENTATION_ITEM('density measure',
POSITIVE_RATIO_MEASURE(7850.),#12407);
#12463=MEASURE_REPRESENTATION_ITEM('density measure',
POSITIVE_RATIO_MEASURE(7850.),#12408);
#12464=MEASURE_REPRESENTATION_ITEM('density measure',
POSITIVE_RATIO_MEASURE(7850.),#12409);
#12465=MEASURE_REPRESENTATION_ITEM('density measure',
POSITIVE_RATIO_MEASURE(7850.),#12410);
#12466=MEASURE_REPRESENTATION_ITEM('density measure',
POSITIVE_RATIO_MEASURE(7850.),#12411);
#12467=MEASURE_REPRESENTATION_ITEM('density measure',
POSITIVE_RATIO_MEASURE(7850.),#12412);
#12468=MEASURE_REPRESENTATION_ITEM('density measure',
POSITIVE_RATIO_MEASURE(7850.),#12413);
#12469=MEASURE_REPRESENTATION_ITEM('density measure',
POSITIVE_RATIO_MEASURE(7850.),#12414);
#12470=MEASURE_REPRESENTATION_ITEM('density measure',
POSITIVE_RATIO_MEASURE(7850.),#12415);
#12471=MEASURE_REPRESENTATION_ITEM('density measure',
POSITIVE_RATIO_MEASURE(7850.),#12416);
#12472=MEASURE_REPRESENTATION_ITEM('density measure',
POSITIVE_RATIO_MEASURE(7850.),#12417);
#12473=MEASURE_REPRESENTATION_ITEM('density measure',
POSITIVE_RATIO_MEASURE(7850.),#12418);
#12474=MEASURE_REPRESENTATION_ITEM('density measure',
POSITIVE_RATIO_MEASURE(7850.),#12419);
#12475=MEASURE_REPRESENTATION_ITEM('density measure',
POSITIVE_RATIO_MEASURE(7850.),#12420);
#12476=MEASURE_REPRESENTATION_ITEM('density measure',
POSITIVE_RATIO_MEASURE(7850.),#12421);
#12477=MEASURE_REPRESENTATION_ITEM('density measure',
POSITIVE_RATIO_MEASURE(7850.),#12422);
#12478=MEASURE_REPRESENTATION_ITEM('density measure',
POSITIVE_RATIO_MEASURE(7850.),#12423);
#12479=MEASURE_REPRESENTATION_ITEM('density measure',
POSITIVE_RATIO_MEASURE(7850.),#12424);
#12480=MEASURE_REPRESENTATION_ITEM('density measure',
POSITIVE_RATIO_MEASURE(7850.),#12425);
#12481=MEASURE_REPRESENTATION_ITEM('density measure',
POSITIVE_RATIO_MEASURE(7850.),#12426);
#12482=MEASURE_REPRESENTATION_ITEM('density measure',
POSITIVE_RATIO_MEASURE(7850.),#12427);
#12483=MEASURE_REPRESENTATION_ITEM('density measure',
POSITIVE_RATIO_MEASURE(7850.),#12428);
#12484=MEASURE_REPRESENTATION_ITEM('density measure',
POSITIVE_RATIO_MEASURE(7850.),#12429);
#12485=MEASURE_REPRESENTATION_ITEM('density measure',
POSITIVE_RATIO_MEASURE(7850.),#12430);
#12486=MEASURE_REPRESENTATION_ITEM('density measure',
POSITIVE_RATIO_MEASURE(7850.),#12431);
#12487=MEASURE_REPRESENTATION_ITEM('density measure',
POSITIVE_RATIO_MEASURE(7850.),#12432);
#12488=MEASURE_REPRESENTATION_ITEM('density measure',
POSITIVE_RATIO_MEASURE(7850.),#12433);
#12489=MEASURE_REPRESENTATION_ITEM('density measure',
POSITIVE_RATIO_MEASURE(7850.),#12434);
#12490=MEASURE_REPRESENTATION_ITEM('density measure',
POSITIVE_RATIO_MEASURE(7850.),#12435);
#12491=PROPERTY_DEFINITION_REPRESENTATION(#12766,#12601);
#12492=PROPERTY_DEFINITION_REPRESENTATION(#12767,#12602);
#12493=PROPERTY_DEFINITION_REPRESENTATION(#12768,#12603);
#12494=PROPERTY_DEFINITION_REPRESENTATION(#12769,#12604);
#12495=PROPERTY_DEFINITION_REPRESENTATION(#12770,#12605);
#12496=PROPERTY_DEFINITION_REPRESENTATION(#12771,#12606);
#12497=PROPERTY_DEFINITION_REPRESENTATION(#12772,#12607);
#12498=PROPERTY_DEFINITION_REPRESENTATION(#12773,#12608);
#12499=PROPERTY_DEFINITION_REPRESENTATION(#12774,#12609);
#12500=PROPERTY_DEFINITION_REPRESENTATION(#12775,#12610);
#12501=PROPERTY_DEFINITION_REPRESENTATION(#12776,#12611);
#12502=PROPERTY_DEFINITION_REPRESENTATION(#12777,#12612);
#12503=PROPERTY_DEFINITION_REPRESENTATION(#12778,#12613);
#12504=PROPERTY_DEFINITION_REPRESENTATION(#12779,#12614);
#12505=PROPERTY_DEFINITION_REPRESENTATION(#12780,#12615);
#12506=PROPERTY_DEFINITION_REPRESENTATION(#12781,#12616);
#12507=PROPERTY_DEFINITION_REPRESENTATION(#12782,#12617);
#12508=PROPERTY_DEFINITION_REPRESENTATION(#12783,#12618);
#12509=PROPERTY_DEFINITION_REPRESENTATION(#12784,#12619);
#12510=PROPERTY_DEFINITION_REPRESENTATION(#12785,#12620);
#12511=PROPERTY_DEFINITION_REPRESENTATION(#12786,#12621);
#12512=PROPERTY_DEFINITION_REPRESENTATION(#12787,#12622);
#12513=PROPERTY_DEFINITION_REPRESENTATION(#12788,#12623);
#12514=PROPERTY_DEFINITION_REPRESENTATION(#12789,#12624);
#12515=PROPERTY_DEFINITION_REPRESENTATION(#12790,#12625);
#12516=PROPERTY_DEFINITION_REPRESENTATION(#12791,#12626);
#12517=PROPERTY_DEFINITION_REPRESENTATION(#12792,#12627);
#12518=PROPERTY_DEFINITION_REPRESENTATION(#12793,#12628);
#12519=PROPERTY_DEFINITION_REPRESENTATION(#12794,#12629);
#12520=PROPERTY_DEFINITION_REPRESENTATION(#12795,#12630);
#12521=PROPERTY_DEFINITION_REPRESENTATION(#12796,#12631);
#12522=PROPERTY_DEFINITION_REPRESENTATION(#12797,#12632);
#12523=PROPERTY_DEFINITION_REPRESENTATION(#12798,#12633);
#12524=PROPERTY_DEFINITION_REPRESENTATION(#12799,#12634);
#12525=PROPERTY_DEFINITION_REPRESENTATION(#12800,#12635);
#12526=PROPERTY_DEFINITION_REPRESENTATION(#12801,#12636);
#12527=PROPERTY_DEFINITION_REPRESENTATION(#12802,#12637);
#12528=PROPERTY_DEFINITION_REPRESENTATION(#12803,#12638);
#12529=PROPERTY_DEFINITION_REPRESENTATION(#12804,#12639);
#12530=PROPERTY_DEFINITION_REPRESENTATION(#12805,#12640);
#12531=PROPERTY_DEFINITION_REPRESENTATION(#12806,#12641);
#12532=PROPERTY_DEFINITION_REPRESENTATION(#12807,#12642);
#12533=PROPERTY_DEFINITION_REPRESENTATION(#12808,#12643);
#12534=PROPERTY_DEFINITION_REPRESENTATION(#12809,#12644);
#12535=PROPERTY_DEFINITION_REPRESENTATION(#12810,#12645);
#12536=PROPERTY_DEFINITION_REPRESENTATION(#12811,#12646);
#12537=PROPERTY_DEFINITION_REPRESENTATION(#12812,#12647);
#12538=PROPERTY_DEFINITION_REPRESENTATION(#12813,#12648);
#12539=PROPERTY_DEFINITION_REPRESENTATION(#12814,#12649);
#12540=PROPERTY_DEFINITION_REPRESENTATION(#12815,#12650);
#12541=PROPERTY_DEFINITION_REPRESENTATION(#12816,#12651);
#12542=PROPERTY_DEFINITION_REPRESENTATION(#12817,#12652);
#12543=PROPERTY_DEFINITION_REPRESENTATION(#12818,#12653);
#12544=PROPERTY_DEFINITION_REPRESENTATION(#12819,#12654);
#12545=PROPERTY_DEFINITION_REPRESENTATION(#12820,#12655);
#12546=PROPERTY_DEFINITION_REPRESENTATION(#12821,#12656);
#12547=PROPERTY_DEFINITION_REPRESENTATION(#12822,#12657);
#12548=PROPERTY_DEFINITION_REPRESENTATION(#12823,#12658);
#12549=PROPERTY_DEFINITION_REPRESENTATION(#12824,#12659);
#12550=PROPERTY_DEFINITION_REPRESENTATION(#12825,#12660);
#12551=PROPERTY_DEFINITION_REPRESENTATION(#12826,#12661);
#12552=PROPERTY_DEFINITION_REPRESENTATION(#12827,#12662);
#12553=PROPERTY_DEFINITION_REPRESENTATION(#12828,#12663);
#12554=PROPERTY_DEFINITION_REPRESENTATION(#12829,#12664);
#12555=PROPERTY_DEFINITION_REPRESENTATION(#12830,#12665);
#12556=PROPERTY_DEFINITION_REPRESENTATION(#12831,#12666);
#12557=PROPERTY_DEFINITION_REPRESENTATION(#12832,#12667);
#12558=PROPERTY_DEFINITION_REPRESENTATION(#12833,#12668);
#12559=PROPERTY_DEFINITION_REPRESENTATION(#12834,#12669);
#12560=PROPERTY_DEFINITION_REPRESENTATION(#12835,#12670);
#12561=PROPERTY_DEFINITION_REPRESENTATION(#12836,#12671);
#12562=PROPERTY_DEFINITION_REPRESENTATION(#12837,#12672);
#12563=PROPERTY_DEFINITION_REPRESENTATION(#12838,#12673);
#12564=PROPERTY_DEFINITION_REPRESENTATION(#12839,#12674);
#12565=PROPERTY_DEFINITION_REPRESENTATION(#12840,#12675);
#12566=PROPERTY_DEFINITION_REPRESENTATION(#12841,#12676);
#12567=PROPERTY_DEFINITION_REPRESENTATION(#12842,#12677);
#12568=PROPERTY_DEFINITION_REPRESENTATION(#12843,#12678);
#12569=PROPERTY_DEFINITION_REPRESENTATION(#12844,#12679);
#12570=PROPERTY_DEFINITION_REPRESENTATION(#12845,#12680);
#12571=PROPERTY_DEFINITION_REPRESENTATION(#12846,#12681);
#12572=PROPERTY_DEFINITION_REPRESENTATION(#12847,#12682);
#12573=PROPERTY_DEFINITION_REPRESENTATION(#12848,#12683);
#12574=PROPERTY_DEFINITION_REPRESENTATION(#12849,#12684);
#12575=PROPERTY_DEFINITION_REPRESENTATION(#12850,#12685);
#12576=PROPERTY_DEFINITION_REPRESENTATION(#12851,#12686);
#12577=PROPERTY_DEFINITION_REPRESENTATION(#12852,#12687);
#12578=PROPERTY_DEFINITION_REPRESENTATION(#12853,#12688);
#12579=PROPERTY_DEFINITION_REPRESENTATION(#12854,#12689);
#12580=PROPERTY_DEFINITION_REPRESENTATION(#12855,#12690);
#12581=PROPERTY_DEFINITION_REPRESENTATION(#12856,#12691);
#12582=PROPERTY_DEFINITION_REPRESENTATION(#12857,#12692);
#12583=PROPERTY_DEFINITION_REPRESENTATION(#12858,#12693);
#12584=PROPERTY_DEFINITION_REPRESENTATION(#12859,#12694);
#12585=PROPERTY_DEFINITION_REPRESENTATION(#12860,#12695);
#12586=PROPERTY_DEFINITION_REPRESENTATION(#12861,#12696);
#12587=PROPERTY_DEFINITION_REPRESENTATION(#12862,#12697);
#12588=PROPERTY_DEFINITION_REPRESENTATION(#12863,#12698);
#12589=PROPERTY_DEFINITION_REPRESENTATION(#12864,#12699);
#12590=PROPERTY_DEFINITION_REPRESENTATION(#12865,#12700);
#12591=PROPERTY_DEFINITION_REPRESENTATION(#12866,#12701);
#12592=PROPERTY_DEFINITION_REPRESENTATION(#12867,#12702);
#12593=PROPERTY_DEFINITION_REPRESENTATION(#12868,#12703);
#12594=PROPERTY_DEFINITION_REPRESENTATION(#12869,#12704);
#12595=PROPERTY_DEFINITION_REPRESENTATION(#12870,#12705);
#12596=PROPERTY_DEFINITION_REPRESENTATION(#12871,#12706);
#12597=PROPERTY_DEFINITION_REPRESENTATION(#12872,#12707);
#12598=PROPERTY_DEFINITION_REPRESENTATION(#12873,#12708);
#12599=PROPERTY_DEFINITION_REPRESENTATION(#12874,#12709);
#12600=PROPERTY_DEFINITION_REPRESENTATION(#12875,#12710);
#12601=REPRESENTATION('material name',(#12711),#23525);
#12602=REPRESENTATION('density',(#12436),#23525);
#12603=REPRESENTATION('material name',(#12712),#23526);
#12604=REPRESENTATION('density',(#12437),#23526);
#12605=REPRESENTATION('material name',(#12713),#23527);
#12606=REPRESENTATION('density',(#12438),#23527);
#12607=REPRESENTATION('material name',(#12714),#23528);
#12608=REPRESENTATION('density',(#12439),#23528);
#12609=REPRESENTATION('material name',(#12715),#23529);
#12610=REPRESENTATION('density',(#12440),#23529);
#12611=REPRESENTATION('material name',(#12716),#23530);
#12612=REPRESENTATION('density',(#12441),#23530);
#12613=REPRESENTATION('material name',(#12717),#23531);
#12614=REPRESENTATION('density',(#12442),#23531);
#12615=REPRESENTATION('material name',(#12718),#23532);
#12616=REPRESENTATION('density',(#12443),#23532);
#12617=REPRESENTATION('material name',(#12719),#23533);
#12618=REPRESENTATION('density',(#12444),#23533);
#12619=REPRESENTATION('material name',(#12720),#23534);
#12620=REPRESENTATION('density',(#12445),#23534);
#12621=REPRESENTATION('material name',(#12721),#23535);
#12622=REPRESENTATION('density',(#12446),#23535);
#12623=REPRESENTATION('material name',(#12722),#23536);
#12624=REPRESENTATION('density',(#12447),#23536);
#12625=REPRESENTATION('material name',(#12723),#23537);
#12626=REPRESENTATION('density',(#12448),#23537);
#12627=REPRESENTATION('material name',(#12724),#23538);
#12628=REPRESENTATION('density',(#12449),#23538);
#12629=REPRESENTATION('material name',(#12725),#23540);
#12630=REPRESENTATION('density',(#12450),#23540);
#12631=REPRESENTATION('material name',(#12726),#23541);
#12632=REPRESENTATION('density',(#12451),#23541);
#12633=REPRESENTATION('material name',(#12727),#23542);
#12634=REPRESENTATION('density',(#12452),#23542);
#12635=REPRESENTATION('material name',(#12728),#23543);
#12636=REPRESENTATION('density',(#12453),#23543);
#12637=REPRESENTATION('material name',(#12729),#23544);
#12638=REPRESENTATION('density',(#12454),#23544);
#12639=REPRESENTATION('material name',(#12730),#23546);
#12640=REPRESENTATION('density',(#12455),#23546);
#12641=REPRESENTATION('material name',(#12731),#23547);
#12642=REPRESENTATION('density',(#12456),#23547);
#12643=REPRESENTATION('material name',(#12732),#23548);
#12644=REPRESENTATION('density',(#12457),#23548);
#12645=REPRESENTATION('material name',(#12733),#23549);
#12646=REPRESENTATION('density',(#12458),#23549);
#12647=REPRESENTATION('material name',(#12734),#23550);
#12648=REPRESENTATION('density',(#12459),#23550);
#12649=REPRESENTATION('material name',(#12735),#23551);
#12650=REPRESENTATION('density',(#12460),#23551);
#12651=REPRESENTATION('material name',(#12736),#23552);
#12652=REPRESENTATION('density',(#12461),#23552);
#12653=REPRESENTATION('material name',(#12737),#23553);
#12654=REPRESENTATION('density',(#12462),#23553);
#12655=REPRESENTATION('material name',(#12738),#23555);
#12656=REPRESENTATION('density',(#12463),#23555);
#12657=REPRESENTATION('material name',(#12739),#23556);
#12658=REPRESENTATION('density',(#12464),#23556);
#12659=REPRESENTATION('material name',(#12740),#23557);
#12660=REPRESENTATION('density',(#12465),#23557);
#12661=REPRESENTATION('material name',(#12741),#23558);
#12662=REPRESENTATION('density',(#12466),#23558);
#12663=REPRESENTATION('material name',(#12742),#23560);
#12664=REPRESENTATION('density',(#12467),#23560);
#12665=REPRESENTATION('material name',(#12743),#23561);
#12666=REPRESENTATION('density',(#12468),#23561);
#12667=REPRESENTATION('material name',(#12744),#23562);
#12668=REPRESENTATION('density',(#12469),#23562);
#12669=REPRESENTATION('material name',(#12745),#23563);
#12670=REPRESENTATION('density',(#12470),#23563);
#12671=REPRESENTATION('material name',(#12746),#23564);
#12672=REPRESENTATION('density',(#12471),#23564);
#12673=REPRESENTATION('material name',(#12747),#23565);
#12674=REPRESENTATION('density',(#12472),#23565);
#12675=REPRESENTATION('material name',(#12748),#23567);
#12676=REPRESENTATION('density',(#12473),#23567);
#12677=REPRESENTATION('material name',(#12749),#23568);
#12678=REPRESENTATION('density',(#12474),#23568);
#12679=REPRESENTATION('material name',(#12750),#23569);
#12680=REPRESENTATION('density',(#12475),#23569);
#12681=REPRESENTATION('material name',(#12751),#23570);
#12682=REPRESENTATION('density',(#12476),#23570);
#12683=REPRESENTATION('material name',(#12752),#23571);
#12684=REPRESENTATION('density',(#12477),#23571);
#12685=REPRESENTATION('material name',(#12753),#23572);
#12686=REPRESENTATION('density',(#12478),#23572);
#12687=REPRESENTATION('material name',(#12754),#23573);
#12688=REPRESENTATION('density',(#12479),#23573);
#12689=REPRESENTATION('material name',(#12755),#23575);
#12690=REPRESENTATION('density',(#12480),#23575);
#12691=REPRESENTATION('material name',(#12756),#23576);
#12692=REPRESENTATION('density',(#12481),#23576);
#12693=REPRESENTATION('material name',(#12757),#23577);
#12694=REPRESENTATION('density',(#12482),#23577);
#12695=REPRESENTATION('material name',(#12758),#23578);
#12696=REPRESENTATION('density',(#12483),#23578);
#12697=REPRESENTATION('material name',(#12759),#23579);
#12698=REPRESENTATION('density',(#12484),#23579);
#12699=REPRESENTATION('material name',(#12760),#23580);
#12700=REPRESENTATION('density',(#12485),#23580);
#12701=REPRESENTATION('material name',(#12761),#23581);
#12702=REPRESENTATION('density',(#12486),#23581);
#12703=REPRESENTATION('material name',(#12762),#23582);
#12704=REPRESENTATION('density',(#12487),#23582);
#12705=REPRESENTATION('material name',(#12763),#23584);
#12706=REPRESENTATION('density',(#12488),#23584);
#12707=REPRESENTATION('material name',(#12764),#23585);
#12708=REPRESENTATION('density',(#12489),#23585);
#12709=REPRESENTATION('material name',(#12765),#23586);
#12710=REPRESENTATION('density',(#12490),#23586);
#12711=DESCRIPTIVE_REPRESENTATION_ITEM('Steel','Steel');
#12712=DESCRIPTIVE_REPRESENTATION_ITEM('Steel','Steel');
#12713=DESCRIPTIVE_REPRESENTATION_ITEM('Steel','Steel');
#12714=DESCRIPTIVE_REPRESENTATION_ITEM('Steel','Steel');
#12715=DESCRIPTIVE_REPRESENTATION_ITEM('Steel','Steel');
#12716=DESCRIPTIVE_REPRESENTATION_ITEM('Steel','Steel');
#12717=DESCRIPTIVE_REPRESENTATION_ITEM('Steel','Steel');
#12718=DESCRIPTIVE_REPRESENTATION_ITEM('Steel','Steel');
#12719=DESCRIPTIVE_REPRESENTATION_ITEM('Steel','Steel');
#12720=DESCRIPTIVE_REPRESENTATION_ITEM('Steel','Steel');
#12721=DESCRIPTIVE_REPRESENTATION_ITEM('Steel','Steel');
#12722=DESCRIPTIVE_REPRESENTATION_ITEM('Steel','Steel');
#12723=DESCRIPTIVE_REPRESENTATION_ITEM('Steel','Steel');
#12724=DESCRIPTIVE_REPRESENTATION_ITEM('Steel','Steel');
#12725=DESCRIPTIVE_REPRESENTATION_ITEM('Steel','Steel');
#12726=DESCRIPTIVE_REPRESENTATION_ITEM('Steel','Steel');
#12727=DESCRIPTIVE_REPRESENTATION_ITEM('Steel','Steel');
#12728=DESCRIPTIVE_REPRESENTATION_ITEM('Steel','Steel');
#12729=DESCRIPTIVE_REPRESENTATION_ITEM('Steel','Steel');
#12730=DESCRIPTIVE_REPRESENTATION_ITEM('Steel','Steel');
#12731=DESCRIPTIVE_REPRESENTATION_ITEM('Steel','Steel');
#12732=DESCRIPTIVE_REPRESENTATION_ITEM('Steel','Steel');
#12733=DESCRIPTIVE_REPRESENTATION_ITEM('Steel','Steel');
#12734=DESCRIPTIVE_REPRESENTATION_ITEM('Steel','Steel');
#12735=DESCRIPTIVE_REPRESENTATION_ITEM('Steel','Steel');
#12736=DESCRIPTIVE_REPRESENTATION_ITEM('Steel','Steel');
#12737=DESCRIPTIVE_REPRESENTATION_ITEM('Steel','Steel');
#12738=DESCRIPTIVE_REPRESENTATION_ITEM('Steel','Steel');
#12739=DESCRIPTIVE_REPRESENTATION_ITEM('Steel','Steel');
#12740=DESCRIPTIVE_REPRESENTATION_ITEM('Steel','Steel');
#12741=DESCRIPTIVE_REPRESENTATION_ITEM('Steel','Steel');
#12742=DESCRIPTIVE_REPRESENTATION_ITEM('Steel','Steel');
#12743=DESCRIPTIVE_REPRESENTATION_ITEM('Steel','Steel');
#12744=DESCRIPTIVE_REPRESENTATION_ITEM('Steel','Steel');
#12745=DESCRIPTIVE_REPRESENTATION_ITEM('Steel','Steel');
#12746=DESCRIPTIVE_REPRESENTATION_ITEM('Steel','Steel');
#12747=DESCRIPTIVE_REPRESENTATION_ITEM('Steel','Steel');
#12748=DESCRIPTIVE_REPRESENTATION_ITEM('Steel','Steel');
#12749=DESCRIPTIVE_REPRESENTATION_ITEM('Steel','Steel');
#12750=DESCRIPTIVE_REPRESENTATION_ITEM('Steel','Steel');
#12751=DESCRIPTIVE_REPRESENTATION_ITEM('Steel','Steel');
#12752=DESCRIPTIVE_REPRESENTATION_ITEM('Steel','Steel');
#12753=DESCRIPTIVE_REPRESENTATION_ITEM('Steel','Steel');
#12754=DESCRIPTIVE_REPRESENTATION_ITEM('Steel','Steel');
#12755=DESCRIPTIVE_REPRESENTATION_ITEM('Steel','Steel');
#12756=DESCRIPTIVE_REPRESENTATION_ITEM('Steel','Steel');
#12757=DESCRIPTIVE_REPRESENTATION_ITEM('Steel','Steel');
#12758=DESCRIPTIVE_REPRESENTATION_ITEM('Steel','Steel');
#12759=DESCRIPTIVE_REPRESENTATION_ITEM('Steel','Steel');
#12760=DESCRIPTIVE_REPRESENTATION_ITEM('Steel','Steel');
#12761=DESCRIPTIVE_REPRESENTATION_ITEM('Steel','Steel');
#12762=DESCRIPTIVE_REPRESENTATION_ITEM('Steel','Steel');
#12763=DESCRIPTIVE_REPRESENTATION_ITEM('Steel','Steel');
#12764=DESCRIPTIVE_REPRESENTATION_ITEM('Steel','Steel');
#12765=DESCRIPTIVE_REPRESENTATION_ITEM('Steel','Steel');
#12766=PROPERTY_DEFINITION('material property','material name',#23892);
#12767=PROPERTY_DEFINITION('material property','density of part',#23892);
#12768=PROPERTY_DEFINITION('material property','material name',#23893);
#12769=PROPERTY_DEFINITION('material property','density of part',#23893);
#12770=PROPERTY_DEFINITION('material property','material name',#23894);
#12771=PROPERTY_DEFINITION('material property','density of part',#23894);
#12772=PROPERTY_DEFINITION('material property','material name',#23895);
#12773=PROPERTY_DEFINITION('material property','density of part',#23895);
#12774=PROPERTY_DEFINITION('material property','material name',#23896);
#12775=PROPERTY_DEFINITION('material property','density of part',#23896);
#12776=PROPERTY_DEFINITION('material property','material name',#23897);
#12777=PROPERTY_DEFINITION('material property','density of part',#23897);
#12778=PROPERTY_DEFINITION('material property','material name',#23898);
#12779=PROPERTY_DEFINITION('material property','density of part',#23898);
#12780=PROPERTY_DEFINITION('material property','material name',#23899);
#12781=PROPERTY_DEFINITION('material property','density of part',#23899);
#12782=PROPERTY_DEFINITION('material property','material name',#23900);
#12783=PROPERTY_DEFINITION('material property','density of part',#23900);
#12784=PROPERTY_DEFINITION('material property','material name',#23901);
#12785=PROPERTY_DEFINITION('material property','density of part',#23901);
#12786=PROPERTY_DEFINITION('material property','material name',#23902);
#12787=PROPERTY_DEFINITION('material property','density of part',#23902);
#12788=PROPERTY_DEFINITION('material property','material name',#23903);
#12789=PROPERTY_DEFINITION('material property','density of part',#23903);
#12790=PROPERTY_DEFINITION('material property','material name',#23904);
#12791=PROPERTY_DEFINITION('material property','density of part',#23904);
#12792=PROPERTY_DEFINITION('material property','material name',#23905);
#12793=PROPERTY_DEFINITION('material property','density of part',#23905);
#12794=PROPERTY_DEFINITION('material property','material name',#23907);
#12795=PROPERTY_DEFINITION('material property','density of part',#23907);
#12796=PROPERTY_DEFINITION('material property','material name',#23908);
#12797=PROPERTY_DEFINITION('material property','density of part',#23908);
#12798=PROPERTY_DEFINITION('material property','material name',#23909);
#12799=PROPERTY_DEFINITION('material property','density of part',#23909);
#12800=PROPERTY_DEFINITION('material property','material name',#23910);
#12801=PROPERTY_DEFINITION('material property','density of part',#23910);
#12802=PROPERTY_DEFINITION('material property','material name',#23911);
#12803=PROPERTY_DEFINITION('material property','density of part',#23911);
#12804=PROPERTY_DEFINITION('material property','material name',#23913);
#12805=PROPERTY_DEFINITION('material property','density of part',#23913);
#12806=PROPERTY_DEFINITION('material property','material name',#23914);
#12807=PROPERTY_DEFINITION('material property','density of part',#23914);
#12808=PROPERTY_DEFINITION('material property','material name',#23915);
#12809=PROPERTY_DEFINITION('material property','density of part',#23915);
#12810=PROPERTY_DEFINITION('material property','material name',#23916);
#12811=PROPERTY_DEFINITION('material property','density of part',#23916);
#12812=PROPERTY_DEFINITION('material property','material name',#23917);
#12813=PROPERTY_DEFINITION('material property','density of part',#23917);
#12814=PROPERTY_DEFINITION('material property','material name',#23918);
#12815=PROPERTY_DEFINITION('material property','density of part',#23918);
#12816=PROPERTY_DEFINITION('material property','material name',#23919);
#12817=PROPERTY_DEFINITION('material property','density of part',#23919);
#12818=PROPERTY_DEFINITION('material property','material name',#23920);
#12819=PROPERTY_DEFINITION('material property','density of part',#23920);
#12820=PROPERTY_DEFINITION('material property','material name',#23922);
#12821=PROPERTY_DEFINITION('material property','density of part',#23922);
#12822=PROPERTY_DEFINITION('material property','material name',#23923);
#12823=PROPERTY_DEFINITION('material property','density of part',#23923);
#12824=PROPERTY_DEFINITION('material property','material name',#23924);
#12825=PROPERTY_DEFINITION('material property','density of part',#23924);
#12826=PROPERTY_DEFINITION('material property','material name',#23925);
#12827=PROPERTY_DEFINITION('material property','density of part',#23925);
#12828=PROPERTY_DEFINITION('material property','material name',#23927);
#12829=PROPERTY_DEFINITION('material property','density of part',#23927);
#12830=PROPERTY_DEFINITION('material property','material name',#23928);
#12831=PROPERTY_DEFINITION('material property','density of part',#23928);
#12832=PROPERTY_DEFINITION('material property','material name',#23929);
#12833=PROPERTY_DEFINITION('material property','density of part',#23929);
#12834=PROPERTY_DEFINITION('material property','material name',#23930);
#12835=PROPERTY_DEFINITION('material property','density of part',#23930);
#12836=PROPERTY_DEFINITION('material property','material name',#23931);
#12837=PROPERTY_DEFINITION('material property','density of part',#23931);
#12838=PROPERTY_DEFINITION('material property','material name',#23932);
#12839=PROPERTY_DEFINITION('material property','density of part',#23932);
#12840=PROPERTY_DEFINITION('material property','material name',#23934);
#12841=PROPERTY_DEFINITION('material property','density of part',#23934);
#12842=PROPERTY_DEFINITION('material property','material name',#23935);
#12843=PROPERTY_DEFINITION('material property','density of part',#23935);
#12844=PROPERTY_DEFINITION('material property','material name',#23936);
#12845=PROPERTY_DEFINITION('material property','density of part',#23936);
#12846=PROPERTY_DEFINITION('material property','material name',#23937);
#12847=PROPERTY_DEFINITION('material property','density of part',#23937);
#12848=PROPERTY_DEFINITION('material property','material name',#23938);
#12849=PROPERTY_DEFINITION('material property','density of part',#23938);
#12850=PROPERTY_DEFINITION('material property','material name',#23939);
#12851=PROPERTY_DEFINITION('material property','density of part',#23939);
#12852=PROPERTY_DEFINITION('material property','material name',#23940);
#12853=PROPERTY_DEFINITION('material property','density of part',#23940);
#12854=PROPERTY_DEFINITION('material property','material name',#23942);
#12855=PROPERTY_DEFINITION('material property','density of part',#23942);
#12856=PROPERTY_DEFINITION('material property','material name',#23943);
#12857=PROPERTY_DEFINITION('material property','density of part',#23943);
#12858=PROPERTY_DEFINITION('material property','material name',#23944);
#12859=PROPERTY_DEFINITION('material property','density of part',#23944);
#12860=PROPERTY_DEFINITION('material property','material name',#23945);
#12861=PROPERTY_DEFINITION('material property','density of part',#23945);
#12862=PROPERTY_DEFINITION('material property','material name',#23946);
#12863=PROPERTY_DEFINITION('material property','density of part',#23946);
#12864=PROPERTY_DEFINITION('material property','material name',#23947);
#12865=PROPERTY_DEFINITION('material property','density of part',#23947);
#12866=PROPERTY_DEFINITION('material property','material name',#23948);
#12867=PROPERTY_DEFINITION('material property','density of part',#23948);
#12868=PROPERTY_DEFINITION('material property','material name',#23949);
#12869=PROPERTY_DEFINITION('material property','density of part',#23949);
#12870=PROPERTY_DEFINITION('material property','material name',#23951);
#12871=PROPERTY_DEFINITION('material property','density of part',#23951);
#12872=PROPERTY_DEFINITION('material property','material name',#23952);
#12873=PROPERTY_DEFINITION('material property','density of part',#23952);
#12874=PROPERTY_DEFINITION('material property','material name',#23953);
#12875=PROPERTY_DEFINITION('material property','density of part',#23953);
#12876=AXIS2_PLACEMENT_3D('',#18550,#14517,#14518);
#12877=AXIS2_PLACEMENT_3D('',#18551,#14519,#14520);
#12878=AXIS2_PLACEMENT_3D('',#18552,#14521,#14522);
#12879=AXIS2_PLACEMENT_3D('',#18553,#14523,#14524);
#12880=AXIS2_PLACEMENT_3D('',#18555,#14525,#14526);
#12881=AXIS2_PLACEMENT_3D('',#18558,#14528,#14529);
#12882=AXIS2_PLACEMENT_3D('',#18559,#14530,#14531);
#12883=AXIS2_PLACEMENT_3D('',#18560,#14532,#14533);
#12884=AXIS2_PLACEMENT_3D('',#18562,#14534,#14535);
#12885=AXIS2_PLACEMENT_3D('',#18565,#14537,#14538);
#12886=AXIS2_PLACEMENT_3D('',#18566,#14539,#14540);
#12887=AXIS2_PLACEMENT_3D('',#18567,#14541,#14542);
#12888=AXIS2_PLACEMENT_3D('',#18569,#14543,#14544);
#12889=AXIS2_PLACEMENT_3D('',#18572,#14546,#14547);
#12890=AXIS2_PLACEMENT_3D('',#18573,#14548,#14549);
#12891=AXIS2_PLACEMENT_3D('',#18574,#14550,#14551);
#12892=AXIS2_PLACEMENT_3D('',#18576,#14552,#14553);
#12893=AXIS2_PLACEMENT_3D('',#18579,#14555,#14556);
#12894=AXIS2_PLACEMENT_3D('',#18580,#14557,#14558);
#12895=AXIS2_PLACEMENT_3D('',#18581,#14559,#14560);
#12896=AXIS2_PLACEMENT_3D('',#18583,#14561,#14562);
#12897=AXIS2_PLACEMENT_3D('',#18586,#14564,#14565);
#12898=AXIS2_PLACEMENT_3D('',#18587,#14566,#14567);
#12899=AXIS2_PLACEMENT_3D('',#18588,#14568,#14569);
#12900=AXIS2_PLACEMENT_3D('',#18590,#14570,#14571);
#12901=AXIS2_PLACEMENT_3D('',#18593,#14573,#14574);
#12902=AXIS2_PLACEMENT_3D('',#18594,#14575,#14576);
#12903=AXIS2_PLACEMENT_3D('',#18595,#14577,#14578);
#12904=AXIS2_PLACEMENT_3D('',#18597,#14579,#14580);
#12905=AXIS2_PLACEMENT_3D('',#18600,#14582,#14583);
#12906=AXIS2_PLACEMENT_3D('',#18601,#14584,#14585);
#12907=AXIS2_PLACEMENT_3D('',#18602,#14586,#14587);
#12908=AXIS2_PLACEMENT_3D('',#18604,#14588,#14589);
#12909=AXIS2_PLACEMENT_3D('',#18607,#14591,#14592);
#12910=AXIS2_PLACEMENT_3D('',#18608,#14593,#14594);
#12911=AXIS2_PLACEMENT_3D('',#18609,#14595,#14596);
#12912=AXIS2_PLACEMENT_3D('',#18611,#14597,#14598);
#12913=AXIS2_PLACEMENT_3D('',#18614,#14600,#14601);
#12914=AXIS2_PLACEMENT_3D('',#18615,#14602,#14603);
#12915=AXIS2_PLACEMENT_3D('',#18616,#14604,#14605);
#12916=AXIS2_PLACEMENT_3D('',#18618,#14606,#14607);
#12917=AXIS2_PLACEMENT_3D('',#18621,#14609,#14610);
#12918=AXIS2_PLACEMENT_3D('',#18622,#14611,#14612);
#12919=AXIS2_PLACEMENT_3D('',#18623,#14613,#14614);
#12920=AXIS2_PLACEMENT_3D('',#18625,#14615,#14616);
#12921=AXIS2_PLACEMENT_3D('',#18628,#14618,#14619);
#12922=AXIS2_PLACEMENT_3D('',#18629,#14620,#14621);
#12923=AXIS2_PLACEMENT_3D('',#18630,#14622,#14623);
#12924=AXIS2_PLACEMENT_3D('',#18632,#14624,#14625);
#12925=AXIS2_PLACEMENT_3D('',#18635,#14627,#14628);
#12926=AXIS2_PLACEMENT_3D('',#18636,#14629,#14630);
#12927=AXIS2_PLACEMENT_3D('',#18637,#14631,#14632);
#12928=AXIS2_PLACEMENT_3D('',#18639,#14633,#14634);
#12929=AXIS2_PLACEMENT_3D('',#18642,#14636,#14637);
#12930=AXIS2_PLACEMENT_3D('',#18643,#14638,#14639);
#12931=AXIS2_PLACEMENT_3D('',#18644,#14640,#14641);
#12932=AXIS2_PLACEMENT_3D('',#18646,#14642,#14643);
#12933=AXIS2_PLACEMENT_3D('',#18649,#14645,#14646);
#12934=AXIS2_PLACEMENT_3D('',#18650,#14647,#14648);
#12935=AXIS2_PLACEMENT_3D('',#18651,#14649,#14650);
#12936=AXIS2_PLACEMENT_3D('',#18660,#14655,#14656);
#12937=AXIS2_PLACEMENT_3D('',#18666,#14660,#14661);
#12938=AXIS2_PLACEMENT_3D('',#18672,#14665,#14666);
#12939=AXIS2_PLACEMENT_3D('',#18675,#14669,#14670);
#12940=AXIS2_PLACEMENT_3D('',#18676,#14671,#14672);
#12941=AXIS2_PLACEMENT_3D('',#18677,#14673,#14674);
#12942=AXIS2_PLACEMENT_3D('',#18678,#14675,#14676);
#12943=AXIS2_PLACEMENT_3D('',#18687,#14681,#14682);
#12944=AXIS2_PLACEMENT_3D('',#18693,#14686,#14687);
#12945=AXIS2_PLACEMENT_3D('',#18699,#14691,#14692);
#12946=AXIS2_PLACEMENT_3D('',#18702,#14695,#14696);
#12947=AXIS2_PLACEMENT_3D('',#18703,#14697,#14698);
#12948=AXIS2_PLACEMENT_3D('',#18704,#14699,#14700);
#12949=AXIS2_PLACEMENT_3D('',#18705,#14701,#14702);
#12950=AXIS2_PLACEMENT_3D('',#18714,#14707,#14708);
#12951=AXIS2_PLACEMENT_3D('',#18720,#14712,#14713);
#12952=AXIS2_PLACEMENT_3D('',#18726,#14717,#14718);
#12953=AXIS2_PLACEMENT_3D('',#18729,#14721,#14722);
#12954=AXIS2_PLACEMENT_3D('',#18730,#14723,#14724);
#12955=AXIS2_PLACEMENT_3D('',#18731,#14725,#14726);
#12956=AXIS2_PLACEMENT_3D('',#18732,#14727,#14728);
#12957=AXIS2_PLACEMENT_3D('',#18734,#14729,#14730);
#12958=AXIS2_PLACEMENT_3D('',#18737,#14732,#14733);
#12959=AXIS2_PLACEMENT_3D('',#18738,#14734,#14735);
#12960=AXIS2_PLACEMENT_3D('',#18740,#14736,#14737);
#12961=AXIS2_PLACEMENT_3D('',#18743,#14739,#14740);
#12962=AXIS2_PLACEMENT_3D('',#18744,#14741,#14742);
#12963=AXIS2_PLACEMENT_3D('',#18746,#14743,#14744);
#12964=AXIS2_PLACEMENT_3D('',#18749,#14746,#14747);
#12965=AXIS2_PLACEMENT_3D('',#18750,#14748,#14749);
#12966=AXIS2_PLACEMENT_3D('',#18752,#14750,#14751);
#12967=AXIS2_PLACEMENT_3D('',#18755,#14753,#14754);
#12968=AXIS2_PLACEMENT_3D('',#18756,#14755,#14756);
#12969=AXIS2_PLACEMENT_3D('',#18758,#14757,#14758);
#12970=AXIS2_PLACEMENT_3D('',#18761,#14760,#14761);
#12971=AXIS2_PLACEMENT_3D('',#18762,#14762,#14763);
#12972=AXIS2_PLACEMENT_3D('',#18764,#14764,#14765);
#12973=AXIS2_PLACEMENT_3D('',#18767,#14767,#14768);
#12974=AXIS2_PLACEMENT_3D('',#18768,#14769,#14770);
#12975=AXIS2_PLACEMENT_3D('',#18770,#14771,#14772);
#12976=AXIS2_PLACEMENT_3D('',#18773,#14774,#14775);
#12977=AXIS2_PLACEMENT_3D('',#18774,#14776,#14777);
#12978=AXIS2_PLACEMENT_3D('',#18776,#14778,#14779);
#12979=AXIS2_PLACEMENT_3D('',#18779,#14781,#14782);
#12980=AXIS2_PLACEMENT_3D('',#18780,#14783,#14784);
#12981=AXIS2_PLACEMENT_3D('',#18782,#14785,#14786);
#12982=AXIS2_PLACEMENT_3D('',#18785,#14788,#14789);
#12983=AXIS2_PLACEMENT_3D('',#18786,#14790,#14791);
#12984=AXIS2_PLACEMENT_3D('',#18795,#14796,#14797);
#12985=AXIS2_PLACEMENT_3D('',#18804,#14802,#14803);
#12986=AXIS2_PLACEMENT_3D('',#18810,#14807,#14808);
#12987=AXIS2_PLACEMENT_3D('',#18816,#14812,#14813);
#12988=AXIS2_PLACEMENT_3D('',#18823,#14818,#14819);
#12989=AXIS2_PLACEMENT_3D('',#18827,#14822,#14823);
#12990=AXIS2_PLACEMENT_3D('',#18832,#14827,#14828);
#12991=AXIS2_PLACEMENT_3D('',#18834,#14830,#14831);
#12992=AXIS2_PLACEMENT_3D('',#18835,#14832,#14833);
#12993=AXIS2_PLACEMENT_3D('',#18836,#14834,#14835);
#12994=AXIS2_PLACEMENT_3D('',#18837,#14836,#14837);
#12995=AXIS2_PLACEMENT_3D('',#18839,#14838,#14839);
#12996=AXIS2_PLACEMENT_3D('',#18842,#14841,#14842);
#12997=AXIS2_PLACEMENT_3D('',#18843,#14843,#14844);
#12998=AXIS2_PLACEMENT_3D('',#18845,#14845,#14846);
#12999=AXIS2_PLACEMENT_3D('',#18848,#14848,#14849);
#13000=AXIS2_PLACEMENT_3D('',#18849,#14850,#14851);
#13001=AXIS2_PLACEMENT_3D('',#18850,#14852,#14853);
#13002=AXIS2_PLACEMENT_3D('',#18851,#14854,#14855);
#13003=AXIS2_PLACEMENT_3D('',#18852,#14856,#14857);
#13004=AXIS2_PLACEMENT_3D('',#18857,#14859,#14860);
#13005=AXIS2_PLACEMENT_3D('',#18860,#14862,#14863);
#13006=AXIS2_PLACEMENT_3D('',#18861,#14864,#14865);
#13007=AXIS2_PLACEMENT_3D('',#18866,#14867,#14868);
#13008=AXIS2_PLACEMENT_3D('',#18869,#14870,#14871);
#13009=AXIS2_PLACEMENT_3D('',#18870,#14872,#14873);
#13010=AXIS2_PLACEMENT_3D('',#18875,#14875,#14876);
#13011=AXIS2_PLACEMENT_3D('',#18878,#14878,#14879);
#13012=AXIS2_PLACEMENT_3D('',#18879,#14880,#14881);
#13013=AXIS2_PLACEMENT_3D('',#18884,#14883,#14884);
#13014=AXIS2_PLACEMENT_3D('',#18887,#14886,#14887);
#13015=AXIS2_PLACEMENT_3D('',#18888,#14888,#14889);
#13016=AXIS2_PLACEMENT_3D('',#18889,#14890,#14891);
#13017=AXIS2_PLACEMENT_3D('',#18890,#14892,#14893);
#13018=AXIS2_PLACEMENT_3D('',#18891,#14894,#14895);
#13019=AXIS2_PLACEMENT_3D('',#18892,#14896,#14897);
#13020=AXIS2_PLACEMENT_3D('',#18894,#14898,#14899);
#13021=AXIS2_PLACEMENT_3D('',#18895,#14900,#14901);
#13022=AXIS2_PLACEMENT_3D('',#18896,#14902,#14903);
#13023=AXIS2_PLACEMENT_3D('',#18897,#14904,#14905);
#13024=AXIS2_PLACEMENT_3D('',#18898,#14906,#14907);
#13025=AXIS2_PLACEMENT_3D('',#18899,#14908,#14909);
#13026=AXIS2_PLACEMENT_3D('',#18900,#14910,#14911);
#13027=AXIS2_PLACEMENT_3D('',#18901,#14912,#14913);
#13028=AXIS2_PLACEMENT_3D('',#18902,#14914,#14915);
#13029=AXIS2_PLACEMENT_3D('',#18903,#14916,#14917);
#13030=AXIS2_PLACEMENT_3D('',#18905,#14918,#14919);
#13031=AXIS2_PLACEMENT_3D('',#18908,#14921,#14922);
#13032=AXIS2_PLACEMENT_3D('',#18909,#14923,#14924);
#13033=AXIS2_PLACEMENT_3D('',#18911,#14925,#14926);
#13034=AXIS2_PLACEMENT_3D('',#18912,#14927,#14928);
#13035=AXIS2_PLACEMENT_3D('',#18914,#14930,#14931);
#13036=AXIS2_PLACEMENT_3D('',#18915,#14932,#14933);
#13037=AXIS2_PLACEMENT_3D('',#18916,#14934,#14935);
#13038=AXIS2_PLACEMENT_3D('',#18921,#14937,#14938);
#13039=AXIS2_PLACEMENT_3D('',#18924,#14940,#14941);
#13040=AXIS2_PLACEMENT_3D('',#18925,#14942,#14943);
#13041=AXIS2_PLACEMENT_3D('',#18930,#14945,#14946);
#13042=AXIS2_PLACEMENT_3D('',#18933,#14948,#14949);
#13043=AXIS2_PLACEMENT_3D('',#18934,#14950,#14951);
#13044=AXIS2_PLACEMENT_3D('',#18939,#14953,#14954);
#13045=AXIS2_PLACEMENT_3D('',#18942,#14956,#14957);
#13046=AXIS2_PLACEMENT_3D('',#18943,#14958,#14959);
#13047=AXIS2_PLACEMENT_3D('',#18948,#14961,#14962);
#13048=AXIS2_PLACEMENT_3D('',#18951,#14964,#14965);
#13049=AXIS2_PLACEMENT_3D('',#18952,#14966,#14967);
#13050=AXIS2_PLACEMENT_3D('',#18953,#14968,#14969);
#13051=AXIS2_PLACEMENT_3D('',#18954,#14970,#14971);
#13052=AXIS2_PLACEMENT_3D('',#18955,#14972,#14973);
#13053=AXIS2_PLACEMENT_3D('',#18956,#14974,#14975);
#13054=AXIS2_PLACEMENT_3D('',#18958,#14976,#14977);
#13055=AXIS2_PLACEMENT_3D('',#18959,#14978,#14979);
#13056=AXIS2_PLACEMENT_3D('',#18960,#14980,#14981);
#13057=AXIS2_PLACEMENT_3D('',#18961,#14982,#14983);
#13058=AXIS2_PLACEMENT_3D('',#18962,#14984,#14985);
#13059=AXIS2_PLACEMENT_3D('',#18963,#14986,#14987);
#13060=AXIS2_PLACEMENT_3D('',#18964,#14988,#14989);
#13061=AXIS2_PLACEMENT_3D('',#18965,#14990,#14991);
#13062=AXIS2_PLACEMENT_3D('',#18966,#14992,#14993);
#13063=AXIS2_PLACEMENT_3D('',#18967,#14994,#14995);
#13064=AXIS2_PLACEMENT_3D('',#18970,#14997,#14998);
#13065=AXIS2_PLACEMENT_3D('',#18971,#14999,#15000);
#13066=AXIS2_PLACEMENT_3D('',#18973,#15001,#15002);
#13067=AXIS2_PLACEMENT_3D('',#18974,#15003,#15004);
#13068=AXIS2_PLACEMENT_3D('',#18976,#15005,#15006);
#13069=AXIS2_PLACEMENT_3D('',#18978,#15008,#15009);
#13070=AXIS2_PLACEMENT_3D('',#18979,#15010,#15011);
#13071=AXIS2_PLACEMENT_3D('',#18980,#15012,#15013);
#13072=AXIS2_PLACEMENT_3D('',#18982,#15014,#15015);
#13073=AXIS2_PLACEMENT_3D('',#18985,#15017,#15018);
#13074=AXIS2_PLACEMENT_3D('',#18986,#15019,#15020);
#13075=AXIS2_PLACEMENT_3D('',#18988,#15021,#15022);
#13076=AXIS2_PLACEMENT_3D('',#18989,#15023,#15024);
#13077=AXIS2_PLACEMENT_3D('',#18991,#15025,#15026);
#13078=AXIS2_PLACEMENT_3D('',#18994,#15028,#15029);
#13079=AXIS2_PLACEMENT_3D('',#18995,#15030,#15031);
#13080=AXIS2_PLACEMENT_3D('',#18997,#15032,#15033);
#13081=AXIS2_PLACEMENT_3D('',#18998,#15034,#15035);
#13082=AXIS2_PLACEMENT_3D('',#19000,#15036,#15037);
#13083=AXIS2_PLACEMENT_3D('',#19002,#15039,#15040);
#13084=AXIS2_PLACEMENT_3D('',#19004,#15041,#15042);
#13085=AXIS2_PLACEMENT_3D('',#19006,#15044,#15045);
#13086=AXIS2_PLACEMENT_3D('',#19008,#15046,#15047);
#13087=AXIS2_PLACEMENT_3D('',#19011,#15049,#15050);
#13088=AXIS2_PLACEMENT_3D('',#19012,#15051,#15052);
#13089=AXIS2_PLACEMENT_3D('',#19021,#15057,#15058);
#13090=AXIS2_PLACEMENT_3D('',#19027,#15062,#15063);
#13091=AXIS2_PLACEMENT_3D('',#19033,#15067,#15068);
#13092=AXIS2_PLACEMENT_3D('',#19036,#15071,#15072);
#13093=AXIS2_PLACEMENT_3D('',#19037,#15073,#15074);
#13094=AXIS2_PLACEMENT_3D('',#19038,#15075,#15076);
#13095=AXIS2_PLACEMENT_3D('',#19039,#15077,#15078);
#13096=AXIS2_PLACEMENT_3D('',#19041,#15079,#15080);
#13097=AXIS2_PLACEMENT_3D('',#19044,#15082,#15083);
#13098=AXIS2_PLACEMENT_3D('',#19045,#15084,#15085);
#13099=AXIS2_PLACEMENT_3D('',#19047,#15086,#15087);
#13100=AXIS2_PLACEMENT_3D('',#19050,#15089,#15090);
#13101=AXIS2_PLACEMENT_3D('',#19051,#15091,#15092);
#13102=AXIS2_PLACEMENT_3D('',#19052,#15093,#15094);
#13103=AXIS2_PLACEMENT_3D('',#19053,#15095,#15096);
#13104=AXIS2_PLACEMENT_3D('',#19054,#15097,#15098);
#13105=AXIS2_PLACEMENT_3D('',#19056,#15099,#15100);
#13106=AXIS2_PLACEMENT_3D('',#19059,#15102,#15103);
#13107=AXIS2_PLACEMENT_3D('',#19060,#15104,#15105);
#13108=AXIS2_PLACEMENT_3D('',#19062,#15106,#15107);
#13109=AXIS2_PLACEMENT_3D('',#19063,#15108,#15109);
#13110=AXIS2_PLACEMENT_3D('',#19065,#15110,#15111);
#13111=AXIS2_PLACEMENT_3D('',#19068,#15113,#15114);
#13112=AXIS2_PLACEMENT_3D('',#19069,#15115,#15116);
#13113=AXIS2_PLACEMENT_3D('',#19071,#15117,#15118);
#13114=AXIS2_PLACEMENT_3D('',#19072,#15119,#15120);
#13115=AXIS2_PLACEMENT_3D('',#19074,#15121,#15122);
#13116=AXIS2_PLACEMENT_3D('',#19076,#15124,#15125);
#13117=AXIS2_PLACEMENT_3D('',#19078,#15126,#15127);
#13118=AXIS2_PLACEMENT_3D('',#19080,#15129,#15130);
#13119=AXIS2_PLACEMENT_3D('',#19082,#15131,#15132);
#13120=AXIS2_PLACEMENT_3D('',#19085,#15134,#15135);
#13121=AXIS2_PLACEMENT_3D('',#19086,#15136,#15137);
#13122=AXIS2_PLACEMENT_3D('',#19095,#15142,#15143);
#13123=AXIS2_PLACEMENT_3D('',#19101,#15147,#15148);
#13124=AXIS2_PLACEMENT_3D('',#19107,#15152,#15153);
#13125=AXIS2_PLACEMENT_3D('',#19110,#15156,#15157);
#13126=AXIS2_PLACEMENT_3D('',#19111,#15158,#15159);
#13127=AXIS2_PLACEMENT_3D('',#19112,#15160,#15161);
#13128=AXIS2_PLACEMENT_3D('',#19113,#15162,#15163);
#13129=AXIS2_PLACEMENT_3D('',#19115,#15164,#15165);
#13130=AXIS2_PLACEMENT_3D('',#19118,#15167,#15168);
#13131=AXIS2_PLACEMENT_3D('',#19119,#15169,#15170);
#13132=AXIS2_PLACEMENT_3D('',#19121,#15171,#15172);
#13133=AXIS2_PLACEMENT_3D('',#19124,#15174,#15175);
#13134=AXIS2_PLACEMENT_3D('',#19125,#15176,#15177);
#13135=AXIS2_PLACEMENT_3D('',#19126,#15178,#15179);
#13136=AXIS2_PLACEMENT_3D('',#19127,#15180,#15181);
#13137=AXIS2_PLACEMENT_3D('',#19128,#15182,#15183);
#13138=AXIS2_PLACEMENT_3D('',#19130,#15184,#15185);
#13139=AXIS2_PLACEMENT_3D('',#19133,#15187,#15188);
#13140=AXIS2_PLACEMENT_3D('',#19134,#15189,#15190);
#13141=AXIS2_PLACEMENT_3D('',#19136,#15191,#15192);
#13142=AXIS2_PLACEMENT_3D('',#19139,#15194,#15195);
#13143=AXIS2_PLACEMENT_3D('',#19140,#15196,#15197);
#13144=AXIS2_PLACEMENT_3D('',#19141,#15198,#15199);
#13145=AXIS2_PLACEMENT_3D('',#19142,#15200,#15201);
#13146=AXIS2_PLACEMENT_3D('',#19143,#15202,#15203);
#13147=AXIS2_PLACEMENT_3D('',#19148,#15205,#15206);
#13148=AXIS2_PLACEMENT_3D('',#19152,#15208,#15209);
#13149=AXIS2_PLACEMENT_3D('',#19159,#15210,#15211);
#13150=AXIS2_PLACEMENT_3D('',#19164,#15213,#15214);
#13151=AXIS2_PLACEMENT_3D('',#19168,#15216,#15217);
#13152=AXIS2_PLACEMENT_3D('',#19201,#15218,#15219);
#13153=AXIS2_PLACEMENT_3D('',#19209,#15220,#15221);
#13154=AXIS2_PLACEMENT_3D('',#19211,#15223,#15224);
#13155=AXIS2_PLACEMENT_3D('',#19212,#15225,#15226);
#13156=AXIS2_PLACEMENT_3D('',#19214,#15227,#15228);
#13157=AXIS2_PLACEMENT_3D('',#19215,#15229,#15230);
#13158=AXIS2_PLACEMENT_3D('',#19249,#15231,#15232);
#13159=AXIS2_PLACEMENT_3D('',#19251,#15234,#15235);
#13160=AXIS2_PLACEMENT_3D('',#19252,#15236,#15237);
#13161=AXIS2_PLACEMENT_3D('',#19254,#15238,#15239);
#13162=AXIS2_PLACEMENT_3D('',#19255,#15240,#15241);
#13163=AXIS2_PLACEMENT_3D('',#19261,#15245,#15246);
#13164=AXIS2_PLACEMENT_3D('',#19267,#15250,#15251);
#13165=AXIS2_PLACEMENT_3D('',#19273,#15255,#15256);
#13166=AXIS2_PLACEMENT_3D('',#19275,#15257,#15258);
#13167=AXIS2_PLACEMENT_3D('',#19277,#15260,#15261);
#13168=AXIS2_PLACEMENT_3D('',#19279,#15262,#15263);
#13169=AXIS2_PLACEMENT_3D('',#19281,#15265,#15266);
#13170=AXIS2_PLACEMENT_3D('',#19284,#15268,#15269);
#13171=AXIS2_PLACEMENT_3D('',#19285,#15270,#15271);
#13172=AXIS2_PLACEMENT_3D('',#19286,#15272,#15273);
#13173=AXIS2_PLACEMENT_3D('',#19294,#15278,#15279);
#13174=AXIS2_PLACEMENT_3D('',#19296,#15281,#15282);
#13175=AXIS2_PLACEMENT_3D('',#19300,#15285,#15286);
#13176=AXIS2_PLACEMENT_3D('',#19304,#15289,#15290);
#13177=AXIS2_PLACEMENT_3D('',#19306,#15292,#15293);
#13178=AXIS2_PLACEMENT_3D('',#19307,#15294,#15295);
#13179=AXIS2_PLACEMENT_3D('',#19308,#15296,#15297);
#13180=AXIS2_PLACEMENT_3D('',#19310,#15298,#15299);
#13181=AXIS2_PLACEMENT_3D('',#19313,#15301,#15302);
#13182=AXIS2_PLACEMENT_3D('',#19314,#15303,#15304);
#13183=AXIS2_PLACEMENT_3D('',#19316,#15305,#15306);
#13184=AXIS2_PLACEMENT_3D('',#19317,#15307,#15308);
#13185=AXIS2_PLACEMENT_3D('',#19319,#15309,#15310);
#13186=AXIS2_PLACEMENT_3D('',#19322,#15312,#15313);
#13187=AXIS2_PLACEMENT_3D('',#19323,#15314,#15315);
#13188=AXIS2_PLACEMENT_3D('',#19325,#15316,#15317);
#13189=AXIS2_PLACEMENT_3D('',#19326,#15318,#15319);
#13190=AXIS2_PLACEMENT_3D('',#19328,#15320,#15321);
#13191=AXIS2_PLACEMENT_3D('',#19331,#15323,#15324);
#13192=AXIS2_PLACEMENT_3D('',#19332,#15325,#15326);
#13193=AXIS2_PLACEMENT_3D('',#19334,#15327,#15328);
#13194=AXIS2_PLACEMENT_3D('',#19335,#15329,#15330);
#13195=AXIS2_PLACEMENT_3D('',#19337,#15331,#15332);
#13196=AXIS2_PLACEMENT_3D('',#19340,#15334,#15335);
#13197=AXIS2_PLACEMENT_3D('',#19341,#15336,#15337);
#13198=AXIS2_PLACEMENT_3D('',#19343,#15338,#15339);
#13199=AXIS2_PLACEMENT_3D('',#19344,#15340,#15341);
#13200=AXIS2_PLACEMENT_3D('',#19346,#15342,#15343);
#13201=AXIS2_PLACEMENT_3D('',#19348,#15345,#15346);
#13202=AXIS2_PLACEMENT_3D('',#19350,#15347,#15348);
#13203=AXIS2_PLACEMENT_3D('',#19352,#15350,#15351);
#13204=AXIS2_PLACEMENT_3D('',#19354,#15352,#15353);
#13205=AXIS2_PLACEMENT_3D('',#19356,#15355,#15356);
#13206=AXIS2_PLACEMENT_3D('',#19358,#15357,#15358);
#13207=AXIS2_PLACEMENT_3D('',#19360,#15360,#15361);
#13208=AXIS2_PLACEMENT_3D('',#19369,#15366,#15367);
#13209=AXIS2_PLACEMENT_3D('',#19375,#15371,#15372);
#13210=AXIS2_PLACEMENT_3D('',#19381,#15376,#15377);
#13211=AXIS2_PLACEMENT_3D('',#19387,#15381,#15382);
#13212=AXIS2_PLACEMENT_3D('',#19393,#15386,#15387);
#13213=AXIS2_PLACEMENT_3D('',#19399,#15391,#15392);
#13214=AXIS2_PLACEMENT_3D('',#19405,#15396,#15397);
#13215=AXIS2_PLACEMENT_3D('',#19411,#15401,#15402);
#13216=AXIS2_PLACEMENT_3D('',#19417,#15406,#15407);
#13217=AXIS2_PLACEMENT_3D('',#19423,#15411,#15412);
#13218=AXIS2_PLACEMENT_3D('',#19429,#15416,#15417);
#13219=AXIS2_PLACEMENT_3D('',#19432,#15420,#15421);
#13220=AXIS2_PLACEMENT_3D('',#19433,#15422,#15423);
#13221=AXIS2_PLACEMENT_3D('',#19434,#15424,#15425);
#13222=AXIS2_PLACEMENT_3D('',#19435,#15426,#15427);
#13223=AXIS2_PLACEMENT_3D('',#19436,#15428,#15429);
#13224=AXIS2_PLACEMENT_3D('',#19439,#15430,#15431);
#13225=AXIS2_PLACEMENT_3D('',#19440,#15432,#15433);
#13226=AXIS2_PLACEMENT_3D('',#19442,#15434,#15435);
#13227=AXIS2_PLACEMENT_3D('',#19444,#15436,#15437);
#13228=AXIS2_PLACEMENT_3D('',#19445,#15438,#15439);
#13229=AXIS2_PLACEMENT_3D('',#19446,#15440,#15441);
#13230=AXIS2_PLACEMENT_3D('',#19449,#15443,#15444);
#13231=AXIS2_PLACEMENT_3D('',#19450,#15445,#15446);
#13232=AXIS2_PLACEMENT_3D('',#19452,#15447,#15448);
#13233=AXIS2_PLACEMENT_3D('',#19455,#15450,#15451);
#13234=AXIS2_PLACEMENT_3D('',#19456,#15452,#15453);
#13235=AXIS2_PLACEMENT_3D('',#19459,#15455,#15456);
#13236=AXIS2_PLACEMENT_3D('',#19460,#15457,#15458);
#13237=AXIS2_PLACEMENT_3D('',#19461,#15459,#15460);
#13238=AXIS2_PLACEMENT_3D('',#19463,#15461,#15462);
#13239=AXIS2_PLACEMENT_3D('',#19465,#15464,#15465);
#13240=AXIS2_PLACEMENT_3D('',#19467,#15466,#15467);
#13241=AXIS2_PLACEMENT_3D('',#19468,#15468,#15469);
#13242=AXIS2_PLACEMENT_3D('',#19470,#15471,#15472);
#13243=AXIS2_PLACEMENT_3D('',#19471,#15473,#15474);
#13244=AXIS2_PLACEMENT_3D('',#19474,#15475,#15476);
#13245=AXIS2_PLACEMENT_3D('',#19475,#15477,#15478);
#13246=AXIS2_PLACEMENT_3D('',#19477,#15479,#15480);
#13247=AXIS2_PLACEMENT_3D('',#19479,#15481,#15482);
#13248=AXIS2_PLACEMENT_3D('',#19480,#15483,#15484);
#13249=AXIS2_PLACEMENT_3D('',#19481,#15485,#15486);
#13250=AXIS2_PLACEMENT_3D('',#19483,#15487,#15488);
#13251=AXIS2_PLACEMENT_3D('',#19485,#15490,#15491);
#13252=AXIS2_PLACEMENT_3D('',#19487,#15492,#15493);
#13253=AXIS2_PLACEMENT_3D('',#19489,#15494,#15495);
#13254=AXIS2_PLACEMENT_3D('',#19490,#15496,#15497);
#13255=AXIS2_PLACEMENT_3D('',#19492,#15498,#15499);
#13256=AXIS2_PLACEMENT_3D('',#19494,#15501,#15502);
#13257=AXIS2_PLACEMENT_3D('',#19496,#15503,#15504);
#13258=AXIS2_PLACEMENT_3D('',#19498,#15506,#15507);
#13259=AXIS2_PLACEMENT_3D('',#19500,#15508,#15509);
#13260=AXIS2_PLACEMENT_3D('',#19502,#15511,#15512);
#13261=AXIS2_PLACEMENT_3D('',#19503,#15513,#15514);
#13262=AXIS2_PLACEMENT_3D('',#19505,#15516,#15517);
#13263=AXIS2_PLACEMENT_3D('',#19506,#15518,#15519);
#13264=AXIS2_PLACEMENT_3D('',#19509,#15520,#15521);
#13265=AXIS2_PLACEMENT_3D('',#19510,#15522,#15523);
#13266=AXIS2_PLACEMENT_3D('',#19513,#15524,#15525);
#13267=AXIS2_PLACEMENT_3D('',#19514,#15526,#15527);
#13268=AXIS2_PLACEMENT_3D('',#19517,#15528,#15529);
#13269=AXIS2_PLACEMENT_3D('',#19518,#15530,#15531);
#13270=AXIS2_PLACEMENT_3D('',#19521,#15532,#15533);
#13271=AXIS2_PLACEMENT_3D('',#19522,#15534,#15535);
#13272=AXIS2_PLACEMENT_3D('',#19525,#15536,#15537);
#13273=AXIS2_PLACEMENT_3D('',#19526,#15538,#15539);
#13274=AXIS2_PLACEMENT_3D('',#19529,#15540,#15541);
#13275=AXIS2_PLACEMENT_3D('',#19530,#15542,#15543);
#13276=AXIS2_PLACEMENT_3D('',#19533,#15544,#15545);
#13277=AXIS2_PLACEMENT_3D('',#19534,#15546,#15547);
#13278=AXIS2_PLACEMENT_3D('',#19537,#15548,#15549);
#13279=AXIS2_PLACEMENT_3D('',#19538,#15550,#15551);
#13280=AXIS2_PLACEMENT_3D('',#19539,#15552,#15553);
#13281=AXIS2_PLACEMENT_3D('',#19565,#15554,#15555);
#13282=AXIS2_PLACEMENT_3D('',#19589,#15556,#15557);
#13283=AXIS2_PLACEMENT_3D('',#19590,#15558,#15559);
#13284=AXIS2_PLACEMENT_3D('',#19592,#15560,#15561);
#13285=AXIS2_PLACEMENT_3D('',#19617,#15562,#15563);
#13286=AXIS2_PLACEMENT_3D('',#19642,#15564,#15565);
#13287=AXIS2_PLACEMENT_3D('',#19658,#15567,#15568);
#13288=AXIS2_PLACEMENT_3D('',#19673,#15569,#15570);
#13289=AXIS2_PLACEMENT_3D('',#19698,#15571,#15572);
#13290=AXIS2_PLACEMENT_3D('',#19723,#15573,#15574);
#13291=AXIS2_PLACEMENT_3D('',#19748,#15575,#15576);
#13292=AXIS2_PLACEMENT_3D('',#19772,#15577,#15578);
#13293=AXIS2_PLACEMENT_3D('',#19773,#15579,#15580);
#13294=AXIS2_PLACEMENT_3D('',#19775,#15581,#15582);
#13295=AXIS2_PLACEMENT_3D('',#19776,#15583,#15584);
#13296=AXIS2_PLACEMENT_3D('',#19777,#15585,#15586);
#13297=AXIS2_PLACEMENT_3D('',#19801,#15587,#15588);
#13298=AXIS2_PLACEMENT_3D('',#19802,#15589,#15590);
#13299=AXIS2_PLACEMENT_3D('',#19804,#15591,#15592);
#13300=AXIS2_PLACEMENT_3D('',#19805,#15593,#15594);
#13301=AXIS2_PLACEMENT_3D('',#19806,#15595,#15596);
#13302=AXIS2_PLACEMENT_3D('',#19830,#15597,#15598);
#13303=AXIS2_PLACEMENT_3D('',#19831,#15599,#15600);
#13304=AXIS2_PLACEMENT_3D('',#19833,#15601,#15602);
#13305=AXIS2_PLACEMENT_3D('',#19834,#15603,#15604);
#13306=AXIS2_PLACEMENT_3D('',#19835,#15605,#15606);
#13307=AXIS2_PLACEMENT_3D('',#19850,#15607,#15608);
#13308=AXIS2_PLACEMENT_3D('',#19863,#15609,#15610);
#13309=AXIS2_PLACEMENT_3D('',#19865,#15611,#15612);
#13310=AXIS2_PLACEMENT_3D('',#19866,#15613,#15614);
#13311=AXIS2_PLACEMENT_3D('',#19867,#15615,#15616);
#13312=AXIS2_PLACEMENT_3D('',#19891,#15617,#15618);
#13313=AXIS2_PLACEMENT_3D('',#19892,#15619,#15620);
#13314=AXIS2_PLACEMENT_3D('',#19894,#15621,#15622);
#13315=AXIS2_PLACEMENT_3D('',#19895,#15623,#15624);
#13316=AXIS2_PLACEMENT_3D('',#19896,#15625,#15626);
#13317=AXIS2_PLACEMENT_3D('',#19920,#15627,#15628);
#13318=AXIS2_PLACEMENT_3D('',#19921,#15629,#15630);
#13319=AXIS2_PLACEMENT_3D('',#19923,#15631,#15632);
#13320=AXIS2_PLACEMENT_3D('',#19924,#15633,#15634);
#13321=AXIS2_PLACEMENT_3D('',#19925,#15635,#15636);
#13322=AXIS2_PLACEMENT_3D('',#19949,#15637,#15638);
#13323=AXIS2_PLACEMENT_3D('',#19950,#15639,#15640);
#13324=AXIS2_PLACEMENT_3D('',#19952,#15641,#15642);
#13325=AXIS2_PLACEMENT_3D('',#19955,#15644,#15645);
#13326=AXIS2_PLACEMENT_3D('',#19979,#15646,#15647);
#13327=AXIS2_PLACEMENT_3D('',#19980,#15648,#15649);
#13328=AXIS2_PLACEMENT_3D('',#19981,#15650,#15651);
#13329=AXIS2_PLACEMENT_3D('',#19982,#15652,#15653);
#13330=AXIS2_PLACEMENT_3D('',#19983,#15654,#15655);
#13331=AXIS2_PLACEMENT_3D('',#19984,#15656,#15657);
#13332=AXIS2_PLACEMENT_3D('',#19985,#15658,#15659);
#13333=AXIS2_PLACEMENT_3D('',#19986,#15660,#15661);
#13334=AXIS2_PLACEMENT_3D('',#19987,#15662,#15663);
#13335=AXIS2_PLACEMENT_3D('',#19989,#15664,#15665);
#13336=AXIS2_PLACEMENT_3D('',#19991,#15666,#15667);
#13337=AXIS2_PLACEMENT_3D('',#19992,#15668,#15669);
#13338=AXIS2_PLACEMENT_3D('',#19994,#15670,#15671);
#13339=AXIS2_PLACEMENT_3D('',#19996,#15673,#15674);
#13340=AXIS2_PLACEMENT_3D('',#19998,#15675,#15676);
#13341=AXIS2_PLACEMENT_3D('',#19999,#15677,#15678);
#13342=AXIS2_PLACEMENT_3D('',#20001,#15680,#15681);
#13343=AXIS2_PLACEMENT_3D('',#20003,#15682,#15683);
#13344=AXIS2_PLACEMENT_3D('',#20005,#15684,#15685);
#13345=AXIS2_PLACEMENT_3D('',#20006,#15686,#15687);
#13346=AXIS2_PLACEMENT_3D('',#20008,#15688,#15689);
#13347=AXIS2_PLACEMENT_3D('',#20010,#15691,#15692);
#13348=AXIS2_PLACEMENT_3D('',#20012,#15693,#15694);
#13349=AXIS2_PLACEMENT_3D('',#20013,#15695,#15696);
#13350=AXIS2_PLACEMENT_3D('',#20015,#15698,#15699);
#13351=AXIS2_PLACEMENT_3D('',#20016,#15700,#15701);
#13352=AXIS2_PLACEMENT_3D('',#20017,#15702,#15703);
#13353=AXIS2_PLACEMENT_3D('',#20018,#15704,#15705);
#13354=AXIS2_PLACEMENT_3D('',#20019,#15706,#15707);
#13355=AXIS2_PLACEMENT_3D('',#20020,#15708,#15709);
#13356=AXIS2_PLACEMENT_3D('',#20021,#15710,#15711);
#13357=AXIS2_PLACEMENT_3D('',#20022,#15712,#15713);
#13358=AXIS2_PLACEMENT_3D('',#20024,#15714,#15715);
#13359=AXIS2_PLACEMENT_3D('',#20027,#15717,#15718);
#13360=AXIS2_PLACEMENT_3D('',#20028,#15719,#15720);
#13361=AXIS2_PLACEMENT_3D('',#20030,#15721,#15722);
#13362=AXIS2_PLACEMENT_3D('',#20033,#15724,#15725);
#13363=AXIS2_PLACEMENT_3D('',#20034,#15726,#15727);
#13364=AXIS2_PLACEMENT_3D('',#20036,#15728,#15729);
#13365=AXIS2_PLACEMENT_3D('',#20039,#15731,#15732);
#13366=AXIS2_PLACEMENT_3D('',#20040,#15733,#15734);
#13367=AXIS2_PLACEMENT_3D('',#20042,#15735,#15736);
#13368=AXIS2_PLACEMENT_3D('',#20045,#15738,#15739);
#13369=AXIS2_PLACEMENT_3D('',#20046,#15740,#15741);
#13370=AXIS2_PLACEMENT_3D('',#20048,#15742,#15743);
#13371=AXIS2_PLACEMENT_3D('',#20051,#15745,#15746);
#13372=AXIS2_PLACEMENT_3D('',#20052,#15747,#15748);
#13373=AXIS2_PLACEMENT_3D('',#20054,#15749,#15750);
#13374=AXIS2_PLACEMENT_3D('',#20057,#15752,#15753);
#13375=AXIS2_PLACEMENT_3D('',#20058,#15754,#15755);
#13376=AXIS2_PLACEMENT_3D('',#20060,#15756,#15757);
#13377=AXIS2_PLACEMENT_3D('',#20063,#15759,#15760);
#13378=AXIS2_PLACEMENT_3D('',#20064,#15761,#15762);
#13379=AXIS2_PLACEMENT_3D('',#20066,#15763,#15764);
#13380=AXIS2_PLACEMENT_3D('',#20069,#15766,#15767);
#13381=AXIS2_PLACEMENT_3D('',#20070,#15768,#15769);
#13382=AXIS2_PLACEMENT_3D('',#20072,#15770,#15771);
#13383=AXIS2_PLACEMENT_3D('',#20075,#15773,#15774);
#13384=AXIS2_PLACEMENT_3D('',#20076,#15775,#15776);
#13385=AXIS2_PLACEMENT_3D('',#20078,#15777,#15778);
#13386=AXIS2_PLACEMENT_3D('',#20081,#15780,#15781);
#13387=AXIS2_PLACEMENT_3D('',#20082,#15782,#15783);
#13388=AXIS2_PLACEMENT_3D('',#20091,#15788,#15789);
#13389=AXIS2_PLACEMENT_3D('',#20097,#15793,#15794);
#13390=AXIS2_PLACEMENT_3D('',#20103,#15798,#15799);
#13391=AXIS2_PLACEMENT_3D('',#20106,#15802,#15803);
#13392=AXIS2_PLACEMENT_3D('',#20107,#15804,#15805);
#13393=AXIS2_PLACEMENT_3D('',#20108,#15806,#15807);
#13394=AXIS2_PLACEMENT_3D('',#20109,#15808,#15809);
#13395=AXIS2_PLACEMENT_3D('',#20111,#15810,#15811);
#13396=AXIS2_PLACEMENT_3D('',#20114,#15813,#15814);
#13397=AXIS2_PLACEMENT_3D('',#20115,#15815,#15816);
#13398=AXIS2_PLACEMENT_3D('',#20117,#15817,#15818);
#13399=AXIS2_PLACEMENT_3D('',#20120,#15820,#15821);
#13400=AXIS2_PLACEMENT_3D('',#20121,#15822,#15823);
#13401=AXIS2_PLACEMENT_3D('',#20123,#15824,#15825);
#13402=AXIS2_PLACEMENT_3D('',#20126,#15827,#15828);
#13403=AXIS2_PLACEMENT_3D('',#20127,#15829,#15830);
#13404=AXIS2_PLACEMENT_3D('',#20129,#15831,#15832);
#13405=AXIS2_PLACEMENT_3D('',#20132,#15834,#15835);
#13406=AXIS2_PLACEMENT_3D('',#20133,#15836,#15837);
#13407=AXIS2_PLACEMENT_3D('',#20135,#15838,#15839);
#13408=AXIS2_PLACEMENT_3D('',#20138,#15841,#15842);
#13409=AXIS2_PLACEMENT_3D('',#20139,#15843,#15844);
#13410=AXIS2_PLACEMENT_3D('',#20143,#15846,#15847);
#13411=AXIS2_PLACEMENT_3D('',#20144,#15848,#15849);
#13412=AXIS2_PLACEMENT_3D('',#20148,#15851,#15852);
#13413=AXIS2_PLACEMENT_3D('',#20150,#15854,#15855);
#13414=AXIS2_PLACEMENT_3D('',#20154,#15857,#15858);
#13415=AXIS2_PLACEMENT_3D('',#20155,#15859,#15860);
#13416=AXIS2_PLACEMENT_3D('',#20159,#15862,#15863);
#13417=AXIS2_PLACEMENT_3D('',#20161,#15865,#15866);
#13418=AXIS2_PLACEMENT_3D('',#20165,#15868,#15869);
#13419=AXIS2_PLACEMENT_3D('',#20166,#15870,#15871);
#13420=AXIS2_PLACEMENT_3D('',#20170,#15873,#15874);
#13421=AXIS2_PLACEMENT_3D('',#20172,#15876,#15877);
#13422=AXIS2_PLACEMENT_3D('',#20176,#15879,#15880);
#13423=AXIS2_PLACEMENT_3D('',#20177,#15881,#15882);
#13424=AXIS2_PLACEMENT_3D('',#20181,#15884,#15885);
#13425=AXIS2_PLACEMENT_3D('',#20183,#15887,#15888);
#13426=AXIS2_PLACEMENT_3D('',#20202,#15899,#15900);
#13427=AXIS2_PLACEMENT_3D('',#20221,#15911,#15912);
#13428=AXIS2_PLACEMENT_3D('',#20223,#15913,#15914);
#13429=AXIS2_PLACEMENT_3D('',#20226,#15916,#15917);
#13430=AXIS2_PLACEMENT_3D('',#20227,#15918,#15919);
#13431=AXIS2_PLACEMENT_3D('',#20229,#15920,#15921);
#13432=AXIS2_PLACEMENT_3D('',#20232,#15923,#15924);
#13433=AXIS2_PLACEMENT_3D('',#20233,#15925,#15926);
#13434=AXIS2_PLACEMENT_3D('',#20235,#15927,#15928);
#13435=AXIS2_PLACEMENT_3D('',#20238,#15930,#15931);
#13436=AXIS2_PLACEMENT_3D('',#20239,#15932,#15933);
#13437=AXIS2_PLACEMENT_3D('',#20241,#15934,#15935);
#13438=AXIS2_PLACEMENT_3D('',#20244,#15937,#15938);
#13439=AXIS2_PLACEMENT_3D('',#20245,#15939,#15940);
#13440=AXIS2_PLACEMENT_3D('',#20248,#15943,#15944);
#13441=AXIS2_PLACEMENT_3D('',#20251,#15947,#15948);
#13442=AXIS2_PLACEMENT_3D('',#20253,#15950,#15951);
#13443=AXIS2_PLACEMENT_3D('',#20255,#15953,#15954);
#13444=AXIS2_PLACEMENT_3D('',#20257,#15956,#15957);
#13445=AXIS2_PLACEMENT_3D('',#20259,#15959,#15960);
#13446=AXIS2_PLACEMENT_3D('',#20260,#15961,#15962);
#13447=AXIS2_PLACEMENT_3D('',#20261,#15963,#15964);
#13448=AXIS2_PLACEMENT_3D('',#20262,#15965,#15966);
#13449=AXIS2_PLACEMENT_3D('',#20264,#15967,#15968);
#13450=AXIS2_PLACEMENT_3D('',#20267,#15970,#15971);
#13451=AXIS2_PLACEMENT_3D('',#20268,#15972,#15973);
#13452=AXIS2_PLACEMENT_3D('',#20270,#15974,#15975);
#13453=AXIS2_PLACEMENT_3D('',#20273,#15977,#15978);
#13454=AXIS2_PLACEMENT_3D('',#20274,#15979,#15980);
#13455=AXIS2_PLACEMENT_3D('',#20275,#15981,#15982);
#13456=AXIS2_PLACEMENT_3D('',#20276,#15983,#15984);
#13457=AXIS2_PLACEMENT_3D('',#20277,#15985,#15986);
#13458=AXIS2_PLACEMENT_3D('',#20282,#15988,#15989);
#13459=AXIS2_PLACEMENT_3D('',#20285,#15991,#15992);
#13460=AXIS2_PLACEMENT_3D('',#20286,#15993,#15994);
#13461=AXIS2_PLACEMENT_3D('',#20291,#15996,#15997);
#13462=AXIS2_PLACEMENT_3D('',#20294,#15999,#16000);
#13463=AXIS2_PLACEMENT_3D('',#20295,#16001,#16002);
#13464=AXIS2_PLACEMENT_3D('',#20300,#16004,#16005);
#13465=AXIS2_PLACEMENT_3D('',#20303,#16007,#16008);
#13466=AXIS2_PLACEMENT_3D('',#20304,#16009,#16010);
#13467=AXIS2_PLACEMENT_3D('',#20309,#16012,#16013);
#13468=AXIS2_PLACEMENT_3D('',#20312,#16015,#16016);
#13469=AXIS2_PLACEMENT_3D('',#20313,#16017,#16018);
#13470=AXIS2_PLACEMENT_3D('',#20314,#16019,#16020);
#13471=AXIS2_PLACEMENT_3D('',#20315,#16021,#16022);
#13472=AXIS2_PLACEMENT_3D('',#20316,#16023,#16024);
#13473=AXIS2_PLACEMENT_3D('',#20317,#16025,#16026);
#13474=AXIS2_PLACEMENT_3D('',#20319,#16027,#16028);
#13475=AXIS2_PLACEMENT_3D('',#20320,#16029,#16030);
#13476=AXIS2_PLACEMENT_3D('',#20321,#16031,#16032);
#13477=AXIS2_PLACEMENT_3D('',#20322,#16033,#16034);
#13478=AXIS2_PLACEMENT_3D('',#20323,#16035,#16036);
#13479=AXIS2_PLACEMENT_3D('',#20324,#16037,#16038);
#13480=AXIS2_PLACEMENT_3D('',#20325,#16039,#16040);
#13481=AXIS2_PLACEMENT_3D('',#20326,#16041,#16042);
#13482=AXIS2_PLACEMENT_3D('',#20327,#16043,#16044);
#13483=AXIS2_PLACEMENT_3D('',#20328,#16045,#16046);
#13484=AXIS2_PLACEMENT_3D('',#20330,#16047,#16048);
#13485=AXIS2_PLACEMENT_3D('',#20333,#16050,#16051);
#13486=AXIS2_PLACEMENT_3D('',#20334,#16052,#16053);
#13487=AXIS2_PLACEMENT_3D('',#20336,#16054,#16055);
#13488=AXIS2_PLACEMENT_3D('',#20337,#16056,#16057);
#13489=AXIS2_PLACEMENT_3D('',#20339,#16059,#16060);
#13490=AXIS2_PLACEMENT_3D('',#20340,#16061,#16062);
#13491=AXIS2_PLACEMENT_3D('',#20341,#16063,#16064);
#13492=AXIS2_PLACEMENT_3D('',#20346,#16066,#16067);
#13493=AXIS2_PLACEMENT_3D('',#20349,#16069,#16070);
#13494=AXIS2_PLACEMENT_3D('',#20350,#16071,#16072);
#13495=AXIS2_PLACEMENT_3D('',#20355,#16074,#16075);
#13496=AXIS2_PLACEMENT_3D('',#20358,#16077,#16078);
#13497=AXIS2_PLACEMENT_3D('',#20359,#16079,#16080);
#13498=AXIS2_PLACEMENT_3D('',#20364,#16082,#16083);
#13499=AXIS2_PLACEMENT_3D('',#20367,#16085,#16086);
#13500=AXIS2_PLACEMENT_3D('',#20368,#16087,#16088);
#13501=AXIS2_PLACEMENT_3D('',#20373,#16090,#16091);
#13502=AXIS2_PLACEMENT_3D('',#20376,#16093,#16094);
#13503=AXIS2_PLACEMENT_3D('',#20377,#16095,#16096);
#13504=AXIS2_PLACEMENT_3D('',#20378,#16097,#16098);
#13505=AXIS2_PLACEMENT_3D('',#20379,#16099,#16100);
#13506=AXIS2_PLACEMENT_3D('',#20380,#16101,#16102);
#13507=AXIS2_PLACEMENT_3D('',#20381,#16103,#16104);
#13508=AXIS2_PLACEMENT_3D('',#20383,#16105,#16106);
#13509=AXIS2_PLACEMENT_3D('',#20384,#16107,#16108);
#13510=AXIS2_PLACEMENT_3D('',#20385,#16109,#16110);
#13511=AXIS2_PLACEMENT_3D('',#20386,#16111,#16112);
#13512=AXIS2_PLACEMENT_3D('',#20387,#16113,#16114);
#13513=AXIS2_PLACEMENT_3D('',#20388,#16115,#16116);
#13514=AXIS2_PLACEMENT_3D('',#20389,#16117,#16118);
#13515=AXIS2_PLACEMENT_3D('',#20390,#16119,#16120);
#13516=AXIS2_PLACEMENT_3D('',#20391,#16121,#16122);
#13517=AXIS2_PLACEMENT_3D('',#20392,#16123,#16124);
#13518=AXIS2_PLACEMENT_3D('',#20395,#16126,#16127);
#13519=AXIS2_PLACEMENT_3D('',#20396,#16128,#16129);
#13520=AXIS2_PLACEMENT_3D('',#20398,#16130,#16131);
#13521=AXIS2_PLACEMENT_3D('',#20399,#16132,#16133);
#13522=AXIS2_PLACEMENT_3D('',#20401,#16134,#16135);
#13523=AXIS2_PLACEMENT_3D('',#20403,#16137,#16138);
#13524=AXIS2_PLACEMENT_3D('',#20404,#16139,#16140);
#13525=AXIS2_PLACEMENT_3D('',#20405,#16141,#16142);
#13526=AXIS2_PLACEMENT_3D('',#20407,#16143,#16144);
#13527=AXIS2_PLACEMENT_3D('',#20410,#16146,#16147);
#13528=AXIS2_PLACEMENT_3D('',#20411,#16148,#16149);
#13529=AXIS2_PLACEMENT_3D('',#20412,#16150,#16151);
#13530=AXIS2_PLACEMENT_3D('',#20414,#16152,#16153);
#13531=AXIS2_PLACEMENT_3D('',#20417,#16155,#16156);
#13532=AXIS2_PLACEMENT_3D('',#20418,#16157,#16158);
#13533=AXIS2_PLACEMENT_3D('',#20419,#16159,#16160);
#13534=AXIS2_PLACEMENT_3D('',#20421,#16161,#16162);
#13535=AXIS2_PLACEMENT_3D('',#20424,#16164,#16165);
#13536=AXIS2_PLACEMENT_3D('',#20425,#16166,#16167);
#13537=AXIS2_PLACEMENT_3D('',#20434,#16172,#16173);
#13538=AXIS2_PLACEMENT_3D('',#20440,#16177,#16178);
#13539=AXIS2_PLACEMENT_3D('',#20446,#16182,#16183);
#13540=AXIS2_PLACEMENT_3D('',#20449,#16186,#16187);
#13541=AXIS2_PLACEMENT_3D('',#20450,#16188,#16189);
#13542=AXIS2_PLACEMENT_3D('',#20451,#16190,#16191);
#13543=AXIS2_PLACEMENT_3D('',#20452,#16192,#16193);
#13544=AXIS2_PLACEMENT_3D('',#20454,#16194,#16195);
#13545=AXIS2_PLACEMENT_3D('',#20455,#16196,#16197);
#13546=AXIS2_PLACEMENT_3D('',#20458,#16199,#16200);
#13547=AXIS2_PLACEMENT_3D('',#20459,#16201,#16202);
#13548=AXIS2_PLACEMENT_3D('',#20460,#16203,#16204);
#13549=AXIS2_PLACEMENT_3D('',#20461,#16205,#16206);
#13550=AXIS2_PLACEMENT_3D('',#20465,#16208,#16209);
#13551=AXIS2_PLACEMENT_3D('',#20466,#16210,#16211);
#13552=AXIS2_PLACEMENT_3D('',#20476,#16212,#16213);
#13553=AXIS2_PLACEMENT_3D('',#20498,#16215,#16216);
#13554=AXIS2_PLACEMENT_3D('',#20499,#16217,#16218);
#13555=AXIS2_PLACEMENT_3D('',#20501,#16220,#16221);
#13556=AXIS2_PLACEMENT_3D('',#20503,#16222,#16223);
#13557=AXIS2_PLACEMENT_3D('',#20507,#16226,#16227);
#13558=AXIS2_PLACEMENT_3D('',#20508,#16228,#16229);
#13559=AXIS2_PLACEMENT_3D('',#20517,#16234,#16235);
#13560=AXIS2_PLACEMENT_3D('',#20523,#16239,#16240);
#13561=AXIS2_PLACEMENT_3D('',#20529,#16244,#16245);
#13562=AXIS2_PLACEMENT_3D('',#20532,#16248,#16249);
#13563=AXIS2_PLACEMENT_3D('',#20533,#16250,#16251);
#13564=AXIS2_PLACEMENT_3D('',#20534,#16252,#16253);
#13565=AXIS2_PLACEMENT_3D('',#20535,#16254,#16255);
#13566=AXIS2_PLACEMENT_3D('',#20536,#16256,#16257);
#13567=AXIS2_PLACEMENT_3D('',#20540,#16259,#16260);
#13568=AXIS2_PLACEMENT_3D('',#20541,#16261,#16262);
#13569=AXIS2_PLACEMENT_3D('',#20545,#16264,#16265);
#13570=AXIS2_PLACEMENT_3D('',#20548,#16267,#16268);
#13571=AXIS2_PLACEMENT_3D('',#20550,#16269,#16270);
#13572=AXIS2_PLACEMENT_3D('',#20552,#16272,#16273);
#13573=AXIS2_PLACEMENT_3D('',#20556,#16275,#16276);
#13574=AXIS2_PLACEMENT_3D('',#20557,#16277,#16278);
#13575=AXIS2_PLACEMENT_3D('',#20561,#16280,#16281);
#13576=AXIS2_PLACEMENT_3D('',#20564,#16283,#16284);
#13577=AXIS2_PLACEMENT_3D('',#20566,#16285,#16286);
#13578=AXIS2_PLACEMENT_3D('',#20568,#16288,#16289);
#13579=AXIS2_PLACEMENT_3D('',#20572,#16291,#16292);
#13580=AXIS2_PLACEMENT_3D('',#20573,#16293,#16294);
#13581=AXIS2_PLACEMENT_3D('',#20577,#16296,#16297);
#13582=AXIS2_PLACEMENT_3D('',#20580,#16299,#16300);
#13583=AXIS2_PLACEMENT_3D('',#20582,#16301,#16302);
#13584=AXIS2_PLACEMENT_3D('',#20584,#16304,#16305);
#13585=AXIS2_PLACEMENT_3D('',#20588,#16307,#16308);
#13586=AXIS2_PLACEMENT_3D('',#20589,#16309,#16310);
#13587=AXIS2_PLACEMENT_3D('',#20593,#16312,#16313);
#13588=AXIS2_PLACEMENT_3D('',#20596,#16315,#16316);
#13589=AXIS2_PLACEMENT_3D('',#20598,#16317,#16318);
#13590=AXIS2_PLACEMENT_3D('',#20600,#16320,#16321);
#13591=AXIS2_PLACEMENT_3D('',#20611,#16328,#16329);
#13592=AXIS2_PLACEMENT_3D('',#20622,#16336,#16337);
#13593=AXIS2_PLACEMENT_3D('',#20641,#16348,#16349);
#13594=AXIS2_PLACEMENT_3D('',#20645,#16352,#16353);
#13595=AXIS2_PLACEMENT_3D('',#20649,#16356,#16357);
#13596=AXIS2_PLACEMENT_3D('',#20653,#16360,#16361);
#13597=AXIS2_PLACEMENT_3D('',#20657,#16364,#16365);
#13598=AXIS2_PLACEMENT_3D('',#20659,#16367,#16368);
#13599=AXIS2_PLACEMENT_3D('',#20663,#16371,#16372);
#13600=AXIS2_PLACEMENT_3D('',#20667,#16375,#16376);
#13601=AXIS2_PLACEMENT_3D('',#20671,#16379,#16380);
#13602=AXIS2_PLACEMENT_3D('',#20675,#16383,#16384);
#13603=AXIS2_PLACEMENT_3D('',#20677,#16386,#16387);
#13604=AXIS2_PLACEMENT_3D('',#20678,#16388,#16389);
#13605=AXIS2_PLACEMENT_3D('',#20679,#16390,#16391);
#13606=AXIS2_PLACEMENT_3D('',#20688,#16396,#16397);
#13607=AXIS2_PLACEMENT_3D('',#20694,#16401,#16402);
#13608=AXIS2_PLACEMENT_3D('',#20700,#16406,#16407);
#13609=AXIS2_PLACEMENT_3D('',#20706,#16411,#16412);
#13610=AXIS2_PLACEMENT_3D('',#20712,#16416,#16417);
#13611=AXIS2_PLACEMENT_3D('',#20718,#16421,#16422);
#13612=AXIS2_PLACEMENT_3D('',#20724,#16426,#16427);
#13613=AXIS2_PLACEMENT_3D('',#20727,#16430,#16431);
#13614=AXIS2_PLACEMENT_3D('',#20728,#16432,#16433);
#13615=AXIS2_PLACEMENT_3D('',#20729,#16434,#16435);
#13616=AXIS2_PLACEMENT_3D('',#20730,#16436,#16437);
#13617=AXIS2_PLACEMENT_3D('',#20739,#16442,#16443);
#13618=AXIS2_PLACEMENT_3D('',#20745,#16447,#16448);
#13619=AXIS2_PLACEMENT_3D('',#20751,#16452,#16453);
#13620=AXIS2_PLACEMENT_3D('',#20757,#16457,#16458);
#13621=AXIS2_PLACEMENT_3D('',#20763,#16462,#16463);
#13622=AXIS2_PLACEMENT_3D('',#20769,#16467,#16468);
#13623=AXIS2_PLACEMENT_3D('',#20775,#16472,#16473);
#13624=AXIS2_PLACEMENT_3D('',#20778,#16476,#16477);
#13625=AXIS2_PLACEMENT_3D('',#20779,#16478,#16479);
#13626=AXIS2_PLACEMENT_3D('',#20780,#16480,#16481);
#13627=AXIS2_PLACEMENT_3D('',#20781,#16482,#16483);
#13628=AXIS2_PLACEMENT_3D('',#20782,#16484,#16485);
#13629=AXIS2_PLACEMENT_3D('',#20783,#16486,#16487);
#13630=AXIS2_PLACEMENT_3D('',#20784,#16488,#16489);
#13631=AXIS2_PLACEMENT_3D('',#20793,#16494,#16495);
#13632=AXIS2_PLACEMENT_3D('',#20799,#16499,#16500);
#13633=AXIS2_PLACEMENT_3D('',#20805,#16504,#16505);
#13634=AXIS2_PLACEMENT_3D('',#20811,#16509,#16510);
#13635=AXIS2_PLACEMENT_3D('',#20817,#16514,#16515);
#13636=AXIS2_PLACEMENT_3D('',#20820,#16518,#16519);
#13637=AXIS2_PLACEMENT_3D('',#20821,#16520,#16521);
#13638=AXIS2_PLACEMENT_3D('',#20822,#16522,#16523);
#13639=AXIS2_PLACEMENT_3D('',#20824,#16524,#16525);
#13640=AXIS2_PLACEMENT_3D('',#20825,#16526,#16527);
#13641=AXIS2_PLACEMENT_3D('',#20827,#16528,#16529);
#13642=AXIS2_PLACEMENT_3D('',#20828,#16530,#16531);
#13643=AXIS2_PLACEMENT_3D('',#20830,#16532,#16533);
#13644=AXIS2_PLACEMENT_3D('',#20832,#16535,#16536);
#13645=AXIS2_PLACEMENT_3D('',#20834,#16537,#16538);
#13646=AXIS2_PLACEMENT_3D('',#20836,#16540,#16541);
#13647=AXIS2_PLACEMENT_3D('',#20838,#16542,#16543);
#13648=AXIS2_PLACEMENT_3D('',#20840,#16545,#16546);
#13649=AXIS2_PLACEMENT_3D('',#20842,#16547,#16548);
#13650=AXIS2_PLACEMENT_3D('',#20843,#16549,#16550);
#13651=AXIS2_PLACEMENT_3D('',#20845,#16551,#16552);
#13652=AXIS2_PLACEMENT_3D('',#20847,#16554,#16555);
#13653=AXIS2_PLACEMENT_3D('',#20849,#16557,#16558);
#13654=AXIS2_PLACEMENT_3D('',#20850,#16559,#16560);
#13655=AXIS2_PLACEMENT_3D('',#20851,#16561,#16562);
#13656=AXIS2_PLACEMENT_3D('',#20854,#16563,#16564);
#13657=AXIS2_PLACEMENT_3D('',#20855,#16565,#16566);
#13658=AXIS2_PLACEMENT_3D('',#20857,#16567,#16568);
#13659=AXIS2_PLACEMENT_3D('',#20859,#16569,#16570);
#13660=AXIS2_PLACEMENT_3D('',#20860,#16571,#16572);
#13661=AXIS2_PLACEMENT_3D('',#20861,#16573,#16574);
#13662=AXIS2_PLACEMENT_3D('',#20864,#16576,#16577);
#13663=AXIS2_PLACEMENT_3D('',#20865,#16578,#16579);
#13664=AXIS2_PLACEMENT_3D('',#20867,#16580,#16581);
#13665=AXIS2_PLACEMENT_3D('',#20870,#16583,#16584);
#13666=AXIS2_PLACEMENT_3D('',#20871,#16585,#16586);
#13667=AXIS2_PLACEMENT_3D('',#20874,#16588,#16589);
#13668=AXIS2_PLACEMENT_3D('',#20875,#16590,#16591);
#13669=AXIS2_PLACEMENT_3D('',#20876,#16592,#16593);
#13670=AXIS2_PLACEMENT_3D('',#20878,#16594,#16595);
#13671=AXIS2_PLACEMENT_3D('',#20880,#16597,#16598);
#13672=AXIS2_PLACEMENT_3D('',#20882,#16599,#16600);
#13673=AXIS2_PLACEMENT_3D('',#20883,#16601,#16602);
#13674=AXIS2_PLACEMENT_3D('',#20885,#16604,#16605);
#13675=AXIS2_PLACEMENT_3D('',#20886,#16606,#16607);
#13676=AXIS2_PLACEMENT_3D('',#20889,#16608,#16609);
#13677=AXIS2_PLACEMENT_3D('',#20890,#16610,#16611);
#13678=AXIS2_PLACEMENT_3D('',#20892,#16612,#16613);
#13679=AXIS2_PLACEMENT_3D('',#20894,#16614,#16615);
#13680=AXIS2_PLACEMENT_3D('',#20895,#16616,#16617);
#13681=AXIS2_PLACEMENT_3D('',#20896,#16618,#16619);
#13682=AXIS2_PLACEMENT_3D('',#20898,#16620,#16621);
#13683=AXIS2_PLACEMENT_3D('',#20900,#16623,#16624);
#13684=AXIS2_PLACEMENT_3D('',#20902,#16625,#16626);
#13685=AXIS2_PLACEMENT_3D('',#20904,#16627,#16628);
#13686=AXIS2_PLACEMENT_3D('',#20905,#16629,#16630);
#13687=AXIS2_PLACEMENT_3D('',#20907,#16631,#16632);
#13688=AXIS2_PLACEMENT_3D('',#20909,#16634,#16635);
#13689=AXIS2_PLACEMENT_3D('',#20911,#16636,#16637);
#13690=AXIS2_PLACEMENT_3D('',#20913,#16639,#16640);
#13691=AXIS2_PLACEMENT_3D('',#20915,#16641,#16642);
#13692=AXIS2_PLACEMENT_3D('',#20917,#16644,#16645);
#13693=AXIS2_PLACEMENT_3D('',#20918,#16646,#16647);
#13694=AXIS2_PLACEMENT_3D('',#20920,#16649,#16650);
#13695=AXIS2_PLACEMENT_3D('',#20921,#16651,#16652);
#13696=AXIS2_PLACEMENT_3D('',#20924,#16653,#16654);
#13697=AXIS2_PLACEMENT_3D('',#20925,#16655,#16656);
#13698=AXIS2_PLACEMENT_3D('',#20928,#16657,#16658);
#13699=AXIS2_PLACEMENT_3D('',#20929,#16659,#16660);
#13700=AXIS2_PLACEMENT_3D('',#20932,#16661,#16662);
#13701=AXIS2_PLACEMENT_3D('',#20933,#16663,#16664);
#13702=AXIS2_PLACEMENT_3D('',#20936,#16665,#16666);
#13703=AXIS2_PLACEMENT_3D('',#20937,#16667,#16668);
#13704=AXIS2_PLACEMENT_3D('',#20940,#16669,#16670);
#13705=AXIS2_PLACEMENT_3D('',#20941,#16671,#16672);
#13706=AXIS2_PLACEMENT_3D('',#20944,#16673,#16674);
#13707=AXIS2_PLACEMENT_3D('',#20945,#16675,#16676);
#13708=AXIS2_PLACEMENT_3D('',#20948,#16677,#16678);
#13709=AXIS2_PLACEMENT_3D('',#20949,#16679,#16680);
#13710=AXIS2_PLACEMENT_3D('',#20950,#16681,#16682);
#13711=AXIS2_PLACEMENT_3D('',#20976,#16683,#16684);
#13712=AXIS2_PLACEMENT_3D('',#21000,#16685,#16686);
#13713=AXIS2_PLACEMENT_3D('',#21001,#16687,#16688);
#13714=AXIS2_PLACEMENT_3D('',#21003,#16689,#16690);
#13715=AXIS2_PLACEMENT_3D('',#21028,#16691,#16692);
#13716=AXIS2_PLACEMENT_3D('',#21053,#16693,#16694);
#13717=AXIS2_PLACEMENT_3D('',#21056,#16696,#16697);
#13718=AXIS2_PLACEMENT_3D('',#21058,#16698,#16699);
#13719=AXIS2_PLACEMENT_3D('',#21083,#16700,#16701);
#13720=AXIS2_PLACEMENT_3D('',#21108,#16702,#16703);
#13721=AXIS2_PLACEMENT_3D('',#21133,#16704,#16705);
#13722=AXIS2_PLACEMENT_3D('',#21157,#16706,#16707);
#13723=AXIS2_PLACEMENT_3D('',#21158,#16708,#16709);
#13724=AXIS2_PLACEMENT_3D('',#21160,#16710,#16711);
#13725=AXIS2_PLACEMENT_3D('',#21161,#16712,#16713);
#13726=AXIS2_PLACEMENT_3D('',#21162,#16714,#16715);
#13727=AXIS2_PLACEMENT_3D('',#21186,#16716,#16717);
#13728=AXIS2_PLACEMENT_3D('',#21187,#16718,#16719);
#13729=AXIS2_PLACEMENT_3D('',#21189,#16720,#16721);
#13730=AXIS2_PLACEMENT_3D('',#21190,#16722,#16723);
#13731=AXIS2_PLACEMENT_3D('',#21191,#16724,#16725);
#13732=AXIS2_PLACEMENT_3D('',#21215,#16726,#16727);
#13733=AXIS2_PLACEMENT_3D('',#21216,#16728,#16729);
#13734=AXIS2_PLACEMENT_3D('',#21218,#16730,#16731);
#13735=AXIS2_PLACEMENT_3D('',#21220,#16732,#16733);
#13736=AXIS2_PLACEMENT_3D('',#21221,#16734,#16735);
#13737=AXIS2_PLACEMENT_3D('',#21222,#16736,#16737);
#13738=AXIS2_PLACEMENT_3D('',#21246,#16738,#16739);
#13739=AXIS2_PLACEMENT_3D('',#21247,#16740,#16741);
#13740=AXIS2_PLACEMENT_3D('',#21249,#16742,#16743);
#13741=AXIS2_PLACEMENT_3D('',#21250,#16744,#16745);
#13742=AXIS2_PLACEMENT_3D('',#21251,#16746,#16747);
#13743=AXIS2_PLACEMENT_3D('',#21275,#16748,#16749);
#13744=AXIS2_PLACEMENT_3D('',#21276,#16750,#16751);
#13745=AXIS2_PLACEMENT_3D('',#21278,#16752,#16753);
#13746=AXIS2_PLACEMENT_3D('',#21279,#16754,#16755);
#13747=AXIS2_PLACEMENT_3D('',#21280,#16756,#16757);
#13748=AXIS2_PLACEMENT_3D('',#21304,#16758,#16759);
#13749=AXIS2_PLACEMENT_3D('',#21305,#16760,#16761);
#13750=AXIS2_PLACEMENT_3D('',#21307,#16762,#16763);
#13751=AXIS2_PLACEMENT_3D('',#21310,#16765,#16766);
#13752=AXIS2_PLACEMENT_3D('',#21334,#16767,#16768);
#13753=AXIS2_PLACEMENT_3D('',#21335,#16769,#16770);
#13754=AXIS2_PLACEMENT_3D('',#21336,#16771,#16772);
#13755=AXIS2_PLACEMENT_3D('',#21337,#16773,#16774);
#13756=AXIS2_PLACEMENT_3D('',#21338,#16775,#16776);
#13757=AXIS2_PLACEMENT_3D('',#21339,#16777,#16778);
#13758=AXIS2_PLACEMENT_3D('',#21340,#16779,#16780);
#13759=AXIS2_PLACEMENT_3D('',#21341,#16781,#16782);
#13760=AXIS2_PLACEMENT_3D('',#21342,#16783,#16784);
#13761=AXIS2_PLACEMENT_3D('',#21344,#16785,#16786);
#13762=AXIS2_PLACEMENT_3D('',#21346,#16787,#16788);
#13763=AXIS2_PLACEMENT_3D('',#21347,#16789,#16790);
#13764=AXIS2_PLACEMENT_3D('',#21349,#16791,#16792);
#13765=AXIS2_PLACEMENT_3D('',#21351,#16794,#16795);
#13766=AXIS2_PLACEMENT_3D('',#21353,#16796,#16797);
#13767=AXIS2_PLACEMENT_3D('',#21354,#16798,#16799);
#13768=AXIS2_PLACEMENT_3D('',#21356,#16801,#16802);
#13769=AXIS2_PLACEMENT_3D('',#21358,#16803,#16804);
#13770=AXIS2_PLACEMENT_3D('',#21360,#16805,#16806);
#13771=AXIS2_PLACEMENT_3D('',#21361,#16807,#16808);
#13772=AXIS2_PLACEMENT_3D('',#21363,#16809,#16810);
#13773=AXIS2_PLACEMENT_3D('',#21365,#16812,#16813);
#13774=AXIS2_PLACEMENT_3D('',#21367,#16814,#16815);
#13775=AXIS2_PLACEMENT_3D('',#21368,#16816,#16817);
#13776=AXIS2_PLACEMENT_3D('',#21370,#16819,#16820);
#13777=AXIS2_PLACEMENT_3D('',#21371,#16821,#16822);
#13778=AXIS2_PLACEMENT_3D('',#21372,#16823,#16824);
#13779=AXIS2_PLACEMENT_3D('',#21373,#16825,#16826);
#13780=AXIS2_PLACEMENT_3D('',#21374,#16827,#16828);
#13781=AXIS2_PLACEMENT_3D('',#21375,#16829,#16830);
#13782=AXIS2_PLACEMENT_3D('',#21376,#16831,#16832);
#13783=AXIS2_PLACEMENT_3D('',#21385,#16837,#16838);
#13784=AXIS2_PLACEMENT_3D('',#21391,#16842,#16843);
#13785=AXIS2_PLACEMENT_3D('',#21397,#16847,#16848);
#13786=AXIS2_PLACEMENT_3D('',#21403,#16852,#16853);
#13787=AXIS2_PLACEMENT_3D('',#21409,#16857,#16858);
#13788=AXIS2_PLACEMENT_3D('',#21412,#16861,#16862);
#13789=AXIS2_PLACEMENT_3D('',#21413,#16863,#16864);
#13790=AXIS2_PLACEMENT_3D('',#21414,#16865,#16866);
#13791=AXIS2_PLACEMENT_3D('',#21416,#16867,#16868);
#13792=AXIS2_PLACEMENT_3D('',#21417,#16869,#16870);
#13793=AXIS2_PLACEMENT_3D('',#21419,#16871,#16872);
#13794=AXIS2_PLACEMENT_3D('',#21420,#16873,#16874);
#13795=AXIS2_PLACEMENT_3D('',#21422,#16875,#16876);
#13796=AXIS2_PLACEMENT_3D('',#21424,#16878,#16879);
#13797=AXIS2_PLACEMENT_3D('',#21426,#16880,#16881);
#13798=AXIS2_PLACEMENT_3D('',#21428,#16883,#16884);
#13799=AXIS2_PLACEMENT_3D('',#21430,#16885,#16886);
#13800=AXIS2_PLACEMENT_3D('',#21432,#16888,#16889);
#13801=AXIS2_PLACEMENT_3D('',#21434,#16890,#16891);
#13802=AXIS2_PLACEMENT_3D('',#21435,#16892,#16893);
#13803=AXIS2_PLACEMENT_3D('',#21437,#16894,#16895);
#13804=AXIS2_PLACEMENT_3D('',#21439,#16897,#16898);
#13805=AXIS2_PLACEMENT_3D('',#21441,#16900,#16901);
#13806=AXIS2_PLACEMENT_3D('',#21442,#16902,#16903);
#13807=AXIS2_PLACEMENT_3D('',#21443,#16904,#16905);
#13808=AXIS2_PLACEMENT_3D('',#21445,#16906,#16907);
#13809=AXIS2_PLACEMENT_3D('',#21448,#16909,#16910);
#13810=AXIS2_PLACEMENT_3D('',#21449,#16911,#16912);
#13811=AXIS2_PLACEMENT_3D('',#21450,#16913,#16914);
#13812=AXIS2_PLACEMENT_3D('',#21452,#16915,#16916);
#13813=AXIS2_PLACEMENT_3D('',#21454,#16917,#16918);
#13814=AXIS2_PLACEMENT_3D('',#21455,#16919,#16920);
#13815=AXIS2_PLACEMENT_3D('',#21457,#16921,#16922);
#13816=AXIS2_PLACEMENT_3D('',#21459,#16923,#16924);
#13817=AXIS2_PLACEMENT_3D('',#21460,#16925,#16926);
#13818=AXIS2_PLACEMENT_3D('',#21462,#16928,#16929);
#13819=AXIS2_PLACEMENT_3D('',#21465,#16931,#16932);
#13820=AXIS2_PLACEMENT_3D('',#21466,#16933,#16934);
#13821=AXIS2_PLACEMENT_3D('',#21468,#16935,#16936);
#13822=AXIS2_PLACEMENT_3D('',#21471,#16938,#16939);
#13823=AXIS2_PLACEMENT_3D('',#21472,#16940,#16941);
#13824=AXIS2_PLACEMENT_3D('',#21473,#16942,#16943);
#13825=AXIS2_PLACEMENT_3D('',#21475,#16944,#16945);
#13826=AXIS2_PLACEMENT_3D('',#21477,#16947,#16948);
#13827=AXIS2_PLACEMENT_3D('',#21478,#16949,#16950);
#13828=AXIS2_PLACEMENT_3D('',#21479,#16951,#16952);
#13829=AXIS2_PLACEMENT_3D('',#21480,#16953,#16954);
#13830=AXIS2_PLACEMENT_3D('',#21482,#16955,#16956);
#13831=AXIS2_PLACEMENT_3D('',#21485,#16958,#16959);
#13832=AXIS2_PLACEMENT_3D('',#21486,#16960,#16961);
#13833=AXIS2_PLACEMENT_3D('',#21488,#16962,#16963);
#13834=AXIS2_PLACEMENT_3D('',#21489,#16964,#16965);
#13835=AXIS2_PLACEMENT_3D('',#21492,#16967,#16968);
#13836=AXIS2_PLACEMENT_3D('',#21493,#16969,#16970);
#13837=AXIS2_PLACEMENT_3D('',#21495,#16971,#16972);
#13838=AXIS2_PLACEMENT_3D('',#21498,#16974,#16975);
#13839=AXIS2_PLACEMENT_3D('',#21499,#16976,#16977);
#13840=AXIS2_PLACEMENT_3D('',#21500,#16978,#16979);
#13841=AXIS2_PLACEMENT_3D('',#21501,#16980,#16981);
#13842=AXIS2_PLACEMENT_3D('',#21502,#16982,#16983);
#13843=AXIS2_PLACEMENT_3D('',#21504,#16984,#16985);
#13844=AXIS2_PLACEMENT_3D('',#21507,#16987,#16988);
#13845=AXIS2_PLACEMENT_3D('',#21508,#16989,#16990);
#13846=AXIS2_PLACEMENT_3D('',#21510,#16991,#16992);
#13847=AXIS2_PLACEMENT_3D('',#21513,#16994,#16995);
#13848=AXIS2_PLACEMENT_3D('',#21514,#16996,#16997);
#13849=AXIS2_PLACEMENT_3D('',#21515,#16998,#16999);
#13850=AXIS2_PLACEMENT_3D('',#21516,#17000,#17001);
#13851=AXIS2_PLACEMENT_3D('',#21517,#17002,#17003);
#13852=AXIS2_PLACEMENT_3D('',#21519,#17004,#17005);
#13853=AXIS2_PLACEMENT_3D('',#21522,#17007,#17008);
#13854=AXIS2_PLACEMENT_3D('',#21523,#17009,#17010);
#13855=AXIS2_PLACEMENT_3D('',#21524,#17011,#17012);
#13856=AXIS2_PLACEMENT_3D('',#21525,#17013,#17014);
#13857=AXIS2_PLACEMENT_3D('',#21526,#17015,#17016);
#13858=AXIS2_PLACEMENT_3D('',#21528,#17017,#17018);
#13859=AXIS2_PLACEMENT_3D('',#21531,#17020,#17021);
#13860=AXIS2_PLACEMENT_3D('',#21532,#17022,#17023);
#13861=AXIS2_PLACEMENT_3D('',#21533,#17024,#17025);
#13862=AXIS2_PLACEMENT_3D('',#21534,#17026,#17027);
#13863=AXIS2_PLACEMENT_3D('',#21535,#17028,#17029);
#13864=AXIS2_PLACEMENT_3D('',#21537,#17030,#17031);
#13865=AXIS2_PLACEMENT_3D('',#21540,#17033,#17034);
#13866=AXIS2_PLACEMENT_3D('',#21541,#17035,#17036);
#13867=AXIS2_PLACEMENT_3D('',#21543,#17037,#17038);
#13868=AXIS2_PLACEMENT_3D('',#21546,#17040,#17041);
#13869=AXIS2_PLACEMENT_3D('',#21547,#17042,#17043);
#13870=AXIS2_PLACEMENT_3D('',#21548,#17044,#17045);
#13871=AXIS2_PLACEMENT_3D('',#21549,#17046,#17047);
#13872=AXIS2_PLACEMENT_3D('',#21550,#17048,#17049);
#13873=AXIS2_PLACEMENT_3D('',#21637,#17051,#17052);
#13874=AXIS2_PLACEMENT_3D('',#21718,#17054,#17055);
#13875=AXIS2_PLACEMENT_3D('',#21720,#17056,#17057);
#13876=AXIS2_PLACEMENT_3D('',#21724,#17060,#17061);
#13877=AXIS2_PLACEMENT_3D('',#21807,#17062,#17063);
#13878=AXIS2_PLACEMENT_3D('',#21847,#17065,#17066);
#13879=AXIS2_PLACEMENT_3D('',#21887,#17068,#17069);
#13880=AXIS2_PLACEMENT_3D('',#21889,#17070,#17071);
#13881=AXIS2_PLACEMENT_3D('',#21893,#17074,#17075);
#13882=AXIS2_PLACEMENT_3D('',#21894,#17076,#17077);
#13883=AXIS2_PLACEMENT_3D('',#21895,#17078,#17079);
#13884=AXIS2_PLACEMENT_3D('',#21897,#17080,#17081);
#13885=AXIS2_PLACEMENT_3D('',#21900,#17082,#17083);
#13886=AXIS2_PLACEMENT_3D('',#21902,#17084,#17085);
#13887=AXIS2_PLACEMENT_3D('',#21904,#17086,#17087);
#13888=AXIS2_PLACEMENT_3D('',#21906,#17088,#17089);
#13889=AXIS2_PLACEMENT_3D('',#21908,#17090,#17091);
#13890=AXIS2_PLACEMENT_3D('',#21910,#17092,#17093);
#13891=AXIS2_PLACEMENT_3D('',#21912,#17094,#17095);
#13892=AXIS2_PLACEMENT_3D('',#21914,#17096,#17097);
#13893=AXIS2_PLACEMENT_3D('',#21916,#17098,#17099);
#13894=AXIS2_PLACEMENT_3D('',#21918,#17100,#17101);
#13895=AXIS2_PLACEMENT_3D('',#21920,#17102,#17103);
#13896=AXIS2_PLACEMENT_3D('',#21922,#17104,#17105);
#13897=AXIS2_PLACEMENT_3D('',#21924,#17106,#17107);
#13898=AXIS2_PLACEMENT_3D('',#21926,#17108,#17109);
#13899=AXIS2_PLACEMENT_3D('',#21928,#17110,#17111);
#13900=AXIS2_PLACEMENT_3D('',#21930,#17112,#17113);
#13901=AXIS2_PLACEMENT_3D('',#21932,#17114,#17115);
#13902=AXIS2_PLACEMENT_3D('',#21934,#17116,#17117);
#13903=AXIS2_PLACEMENT_3D('',#21936,#17118,#17119);
#13904=AXIS2_PLACEMENT_3D('',#21938,#17120,#17121);
#13905=AXIS2_PLACEMENT_3D('',#21940,#17122,#17123);
#13906=AXIS2_PLACEMENT_3D('',#21942,#17124,#17125);
#13907=AXIS2_PLACEMENT_3D('',#21944,#17126,#17127);
#13908=AXIS2_PLACEMENT_3D('',#21946,#17128,#17129);
#13909=AXIS2_PLACEMENT_3D('',#21948,#17130,#17131);
#13910=AXIS2_PLACEMENT_3D('',#21950,#17132,#17133);
#13911=AXIS2_PLACEMENT_3D('',#21952,#17134,#17135);
#13912=AXIS2_PLACEMENT_3D('',#21954,#17136,#17137);
#13913=AXIS2_PLACEMENT_3D('',#21956,#17138,#17139);
#13914=AXIS2_PLACEMENT_3D('',#21958,#17140,#17141);
#13915=AXIS2_PLACEMENT_3D('',#21960,#17142,#17143);
#13916=AXIS2_PLACEMENT_3D('',#21962,#17144,#17145);
#13917=AXIS2_PLACEMENT_3D('',#21964,#17146,#17147);
#13918=AXIS2_PLACEMENT_3D('',#21966,#17148,#17149);
#13919=AXIS2_PLACEMENT_3D('',#21968,#17150,#17151);
#13920=AXIS2_PLACEMENT_3D('',#21970,#17152,#17153);
#13921=AXIS2_PLACEMENT_3D('',#21972,#17154,#17155);
#13922=AXIS2_PLACEMENT_3D('',#21974,#17156,#17157);
#13923=AXIS2_PLACEMENT_3D('',#21976,#17158,#17159);
#13924=AXIS2_PLACEMENT_3D('',#21977,#17160,#17161);
#13925=AXIS2_PLACEMENT_3D('',#21978,#17162,#17163);
#13926=AXIS2_PLACEMENT_3D('',#21980,#17164,#17165);
#13927=AXIS2_PLACEMENT_3D('',#21982,#17167,#17168);
#13928=AXIS2_PLACEMENT_3D('',#21983,#17169,#17170);
#13929=AXIS2_PLACEMENT_3D('',#21985,#17171,#17172);
#13930=AXIS2_PLACEMENT_3D('',#21988,#17173,#17174);
#13931=AXIS2_PLACEMENT_3D('',#21990,#17175,#17176);
#13932=AXIS2_PLACEMENT_3D('',#21992,#17177,#17178);
#13933=AXIS2_PLACEMENT_3D('',#21994,#17179,#17180);
#13934=AXIS2_PLACEMENT_3D('',#21996,#17181,#17182);
#13935=AXIS2_PLACEMENT_3D('',#21998,#17183,#17184);
#13936=AXIS2_PLACEMENT_3D('',#22000,#17185,#17186);
#13937=AXIS2_PLACEMENT_3D('',#22002,#17187,#17188);
#13938=AXIS2_PLACEMENT_3D('',#22004,#17189,#17190);
#13939=AXIS2_PLACEMENT_3D('',#22006,#17191,#17192);
#13940=AXIS2_PLACEMENT_3D('',#22008,#17193,#17194);
#13941=AXIS2_PLACEMENT_3D('',#22010,#17195,#17196);
#13942=AXIS2_PLACEMENT_3D('',#22012,#17197,#17198);
#13943=AXIS2_PLACEMENT_3D('',#22014,#17199,#17200);
#13944=AXIS2_PLACEMENT_3D('',#22016,#17201,#17202);
#13945=AXIS2_PLACEMENT_3D('',#22018,#17203,#17204);
#13946=AXIS2_PLACEMENT_3D('',#22020,#17205,#17206);
#13947=AXIS2_PLACEMENT_3D('',#22022,#17207,#17208);
#13948=AXIS2_PLACEMENT_3D('',#22024,#17209,#17210);
#13949=AXIS2_PLACEMENT_3D('',#22026,#17211,#17212);
#13950=AXIS2_PLACEMENT_3D('',#22028,#17213,#17214);
#13951=AXIS2_PLACEMENT_3D('',#22030,#17215,#17216);
#13952=AXIS2_PLACEMENT_3D('',#22032,#17217,#17218);
#13953=AXIS2_PLACEMENT_3D('',#22034,#17219,#17220);
#13954=AXIS2_PLACEMENT_3D('',#22036,#17221,#17222);
#13955=AXIS2_PLACEMENT_3D('',#22038,#17223,#17224);
#13956=AXIS2_PLACEMENT_3D('',#22040,#17225,#17226);
#13957=AXIS2_PLACEMENT_3D('',#22042,#17227,#17228);
#13958=AXIS2_PLACEMENT_3D('',#22044,#17229,#17230);
#13959=AXIS2_PLACEMENT_3D('',#22046,#17231,#17232);
#13960=AXIS2_PLACEMENT_3D('',#22048,#17233,#17234);
#13961=AXIS2_PLACEMENT_3D('',#22050,#17235,#17236);
#13962=AXIS2_PLACEMENT_3D('',#22052,#17237,#17238);
#13963=AXIS2_PLACEMENT_3D('',#22054,#17239,#17240);
#13964=AXIS2_PLACEMENT_3D('',#22056,#17241,#17242);
#13965=AXIS2_PLACEMENT_3D('',#22058,#17243,#17244);
#13966=AXIS2_PLACEMENT_3D('',#22060,#17245,#17246);
#13967=AXIS2_PLACEMENT_3D('',#22062,#17247,#17248);
#13968=AXIS2_PLACEMENT_3D('',#22064,#17249,#17250);
#13969=AXIS2_PLACEMENT_3D('',#22065,#17251,#17252);
#13970=AXIS2_PLACEMENT_3D('',#22066,#17253,#17254);
#13971=AXIS2_PLACEMENT_3D('',#22068,#17255,#17256);
#13972=AXIS2_PLACEMENT_3D('',#22070,#17258,#17259);
#13973=AXIS2_PLACEMENT_3D('',#22071,#17260,#17261);
#13974=AXIS2_PLACEMENT_3D('',#22074,#17264,#17265);
#13975=AXIS2_PLACEMENT_3D('',#22076,#17267,#17268);
#13976=AXIS2_PLACEMENT_3D('',#22078,#17270,#17271);
#13977=AXIS2_PLACEMENT_3D('',#22080,#17273,#17274);
#13978=AXIS2_PLACEMENT_3D('',#22082,#17276,#17277);
#13979=AXIS2_PLACEMENT_3D('',#22084,#17279,#17280);
#13980=AXIS2_PLACEMENT_3D('',#22086,#17282,#17283);
#13981=AXIS2_PLACEMENT_3D('',#22088,#17285,#17286);
#13982=AXIS2_PLACEMENT_3D('',#22090,#17288,#17289);
#13983=AXIS2_PLACEMENT_3D('',#22092,#17291,#17292);
#13984=AXIS2_PLACEMENT_3D('',#22094,#17294,#17295);
#13985=AXIS2_PLACEMENT_3D('',#22096,#17297,#17298);
#13986=AXIS2_PLACEMENT_3D('',#22098,#17300,#17301);
#13987=AXIS2_PLACEMENT_3D('',#22100,#17303,#17304);
#13988=AXIS2_PLACEMENT_3D('',#22102,#17306,#17307);
#13989=AXIS2_PLACEMENT_3D('',#22104,#17309,#17310);
#13990=AXIS2_PLACEMENT_3D('',#22106,#17312,#17313);
#13991=AXIS2_PLACEMENT_3D('',#22108,#17315,#17316);
#13992=AXIS2_PLACEMENT_3D('',#22110,#17318,#17319);
#13993=AXIS2_PLACEMENT_3D('',#22112,#17321,#17322);
#13994=AXIS2_PLACEMENT_3D('',#22114,#17324,#17325);
#13995=AXIS2_PLACEMENT_3D('',#22116,#17327,#17328);
#13996=AXIS2_PLACEMENT_3D('',#22118,#17330,#17331);
#13997=AXIS2_PLACEMENT_3D('',#22120,#17333,#17334);
#13998=AXIS2_PLACEMENT_3D('',#22122,#17336,#17337);
#13999=AXIS2_PLACEMENT_3D('',#22124,#17339,#17340);
#14000=AXIS2_PLACEMENT_3D('',#22126,#17342,#17343);
#14001=AXIS2_PLACEMENT_3D('',#22128,#17345,#17346);
#14002=AXIS2_PLACEMENT_3D('',#22130,#17348,#17349);
#14003=AXIS2_PLACEMENT_3D('',#22132,#17351,#17352);
#14004=AXIS2_PLACEMENT_3D('',#22134,#17354,#17355);
#14005=AXIS2_PLACEMENT_3D('',#22136,#17357,#17358);
#14006=AXIS2_PLACEMENT_3D('',#22138,#17360,#17361);
#14007=AXIS2_PLACEMENT_3D('',#22140,#17363,#17364);
#14008=AXIS2_PLACEMENT_3D('',#22142,#17366,#17367);
#14009=AXIS2_PLACEMENT_3D('',#22144,#17369,#17370);
#14010=AXIS2_PLACEMENT_3D('',#22146,#17372,#17373);
#14011=AXIS2_PLACEMENT_3D('',#22148,#17375,#17376);
#14012=AXIS2_PLACEMENT_3D('',#22150,#17378,#17379);
#14013=AXIS2_PLACEMENT_3D('',#22151,#17380,#17381);
#14014=AXIS2_PLACEMENT_3D('',#22152,#17382,#17383);
#14015=AXIS2_PLACEMENT_3D('',#22153,#17384,#17385);
#14016=AXIS2_PLACEMENT_3D('',#22155,#17386,#17387);
#14017=AXIS2_PLACEMENT_3D('',#22158,#17389,#17390);
#14018=AXIS2_PLACEMENT_3D('',#22159,#17391,#17392);
#14019=AXIS2_PLACEMENT_3D('',#22160,#17393,#17394);
#14020=AXIS2_PLACEMENT_3D('',#22162,#17395,#17396);
#14021=AXIS2_PLACEMENT_3D('',#22164,#17397,#17398);
#14022=AXIS2_PLACEMENT_3D('',#22165,#17399,#17400);
#14023=AXIS2_PLACEMENT_3D('',#22167,#17401,#17402);
#14024=AXIS2_PLACEMENT_3D('',#22169,#17403,#17404);
#14025=AXIS2_PLACEMENT_3D('',#22170,#17405,#17406);
#14026=AXIS2_PLACEMENT_3D('',#22172,#17408,#17409);
#14027=AXIS2_PLACEMENT_3D('',#22175,#17411,#17412);
#14028=AXIS2_PLACEMENT_3D('',#22176,#17413,#17414);
#14029=AXIS2_PLACEMENT_3D('',#22177,#17415,#17416);
#14030=AXIS2_PLACEMENT_3D('',#22179,#17417,#17418);
#14031=AXIS2_PLACEMENT_3D('',#22181,#17420,#17421);
#14032=AXIS2_PLACEMENT_3D('',#22182,#17422,#17423);
#14033=AXIS2_PLACEMENT_3D('',#22183,#17424,#17425);
#14034=AXIS2_PLACEMENT_3D('',#22185,#17426,#17427);
#14035=AXIS2_PLACEMENT_3D('',#22188,#17429,#17430);
#14036=AXIS2_PLACEMENT_3D('',#22189,#17431,#17432);
#14037=AXIS2_PLACEMENT_3D('',#22191,#17433,#17434);
#14038=AXIS2_PLACEMENT_3D('',#22194,#17436,#17437);
#14039=AXIS2_PLACEMENT_3D('',#22195,#17438,#17439);
#14040=AXIS2_PLACEMENT_3D('',#22196,#17440,#17441);
#14041=AXIS2_PLACEMENT_3D('',#22197,#17442,#17443);
#14042=AXIS2_PLACEMENT_3D('',#22198,#17444,#17445);
#14043=AXIS2_PLACEMENT_3D('',#22200,#17446,#17447);
#14044=AXIS2_PLACEMENT_3D('',#22203,#17449,#17450);
#14045=AXIS2_PLACEMENT_3D('',#22204,#17451,#17452);
#14046=AXIS2_PLACEMENT_3D('',#22206,#17453,#17454);
#14047=AXIS2_PLACEMENT_3D('',#22209,#17456,#17457);
#14048=AXIS2_PLACEMENT_3D('',#22210,#17458,#17459);
#14049=AXIS2_PLACEMENT_3D('',#22211,#17460,#17461);
#14050=AXIS2_PLACEMENT_3D('',#22212,#17462,#17463);
#14051=AXIS2_PLACEMENT_3D('',#22213,#17464,#17465);
#14052=AXIS2_PLACEMENT_3D('',#22215,#17466,#17467);
#14053=AXIS2_PLACEMENT_3D('',#22218,#17469,#17470);
#14054=AXIS2_PLACEMENT_3D('',#22219,#17471,#17472);
#14055=AXIS2_PLACEMENT_3D('',#22220,#17473,#17474);
#14056=AXIS2_PLACEMENT_3D('',#22221,#17475,#17476);
#14057=AXIS2_PLACEMENT_3D('',#22222,#17477,#17478);
#14058=AXIS2_PLACEMENT_3D('',#22224,#17479,#17480);
#14059=AXIS2_PLACEMENT_3D('',#22227,#17482,#17483);
#14060=AXIS2_PLACEMENT_3D('',#22228,#17484,#17485);
#14061=AXIS2_PLACEMENT_3D('',#22229,#17486,#17487);
#14062=AXIS2_PLACEMENT_3D('',#22230,#17488,#17489);
#14063=AXIS2_PLACEMENT_3D('',#22231,#17490,#17491);
#14064=AXIS2_PLACEMENT_3D('',#22233,#17492,#17493);
#14065=AXIS2_PLACEMENT_3D('',#22236,#17495,#17496);
#14066=AXIS2_PLACEMENT_3D('',#22237,#17497,#17498);
#14067=AXIS2_PLACEMENT_3D('',#22239,#17499,#17500);
#14068=AXIS2_PLACEMENT_3D('',#22242,#17502,#17503);
#14069=AXIS2_PLACEMENT_3D('',#22243,#17504,#17505);
#14070=AXIS2_PLACEMENT_3D('',#22244,#17506,#17507);
#14071=AXIS2_PLACEMENT_3D('',#22245,#17508,#17509);
#14072=AXIS2_PLACEMENT_3D('',#22246,#17510,#17511);
#14073=AXIS2_PLACEMENT_3D('',#22333,#17513,#17514);
#14074=AXIS2_PLACEMENT_3D('',#22414,#17516,#17517);
#14075=AXIS2_PLACEMENT_3D('',#22416,#17518,#17519);
#14076=AXIS2_PLACEMENT_3D('',#22420,#17522,#17523);
#14077=AXIS2_PLACEMENT_3D('',#22503,#17524,#17525);
#14078=AXIS2_PLACEMENT_3D('',#22543,#17527,#17528);
#14079=AXIS2_PLACEMENT_3D('',#22583,#17530,#17531);
#14080=AXIS2_PLACEMENT_3D('',#22585,#17532,#17533);
#14081=AXIS2_PLACEMENT_3D('',#22589,#17536,#17537);
#14082=AXIS2_PLACEMENT_3D('',#22590,#17538,#17539);
#14083=AXIS2_PLACEMENT_3D('',#22591,#17540,#17541);
#14084=AXIS2_PLACEMENT_3D('',#22593,#17542,#17543);
#14085=AXIS2_PLACEMENT_3D('',#22596,#17544,#17545);
#14086=AXIS2_PLACEMENT_3D('',#22598,#17546,#17547);
#14087=AXIS2_PLACEMENT_3D('',#22600,#17548,#17549);
#14088=AXIS2_PLACEMENT_3D('',#22602,#17550,#17551);
#14089=AXIS2_PLACEMENT_3D('',#22604,#17552,#17553);
#14090=AXIS2_PLACEMENT_3D('',#22606,#17554,#17555);
#14091=AXIS2_PLACEMENT_3D('',#22608,#17556,#17557);
#14092=AXIS2_PLACEMENT_3D('',#22610,#17558,#17559);
#14093=AXIS2_PLACEMENT_3D('',#22612,#17560,#17561);
#14094=AXIS2_PLACEMENT_3D('',#22614,#17562,#17563);
#14095=AXIS2_PLACEMENT_3D('',#22616,#17564,#17565);
#14096=AXIS2_PLACEMENT_3D('',#22618,#17566,#17567);
#14097=AXIS2_PLACEMENT_3D('',#22620,#17568,#17569);
#14098=AXIS2_PLACEMENT_3D('',#22622,#17570,#17571);
#14099=AXIS2_PLACEMENT_3D('',#22624,#17572,#17573);
#14100=AXIS2_PLACEMENT_3D('',#22626,#17574,#17575);
#14101=AXIS2_PLACEMENT_3D('',#22628,#17576,#17577);
#14102=AXIS2_PLACEMENT_3D('',#22630,#17578,#17579);
#14103=AXIS2_PLACEMENT_3D('',#22632,#17580,#17581);
#14104=AXIS2_PLACEMENT_3D('',#22634,#17582,#17583);
#14105=AXIS2_PLACEMENT_3D('',#22636,#17584,#17585);
#14106=AXIS2_PLACEMENT_3D('',#22638,#17586,#17587);
#14107=AXIS2_PLACEMENT_3D('',#22640,#17588,#17589);
#14108=AXIS2_PLACEMENT_3D('',#22642,#17590,#17591);
#14109=AXIS2_PLACEMENT_3D('',#22644,#17592,#17593);
#14110=AXIS2_PLACEMENT_3D('',#22646,#17594,#17595);
#14111=AXIS2_PLACEMENT_3D('',#22648,#17596,#17597);
#14112=AXIS2_PLACEMENT_3D('',#22650,#17598,#17599);
#14113=AXIS2_PLACEMENT_3D('',#22652,#17600,#17601);
#14114=AXIS2_PLACEMENT_3D('',#22654,#17602,#17603);
#14115=AXIS2_PLACEMENT_3D('',#22656,#17604,#17605);
#14116=AXIS2_PLACEMENT_3D('',#22658,#17606,#17607);
#14117=AXIS2_PLACEMENT_3D('',#22660,#17608,#17609);
#14118=AXIS2_PLACEMENT_3D('',#22662,#17610,#17611);
#14119=AXIS2_PLACEMENT_3D('',#22664,#17612,#17613);
#14120=AXIS2_PLACEMENT_3D('',#22666,#17614,#17615);
#14121=AXIS2_PLACEMENT_3D('',#22668,#17616,#17617);
#14122=AXIS2_PLACEMENT_3D('',#22670,#17618,#17619);
#14123=AXIS2_PLACEMENT_3D('',#22672,#17620,#17621);
#14124=AXIS2_PLACEMENT_3D('',#22674,#17622,#17623);
#14125=AXIS2_PLACEMENT_3D('',#22676,#17624,#17625);
#14126=AXIS2_PLACEMENT_3D('',#22678,#17626,#17627);
#14127=AXIS2_PLACEMENT_3D('',#22680,#17628,#17629);
#14128=AXIS2_PLACEMENT_3D('',#22682,#17630,#17631);
#14129=AXIS2_PLACEMENT_3D('',#22684,#17632,#17633);
#14130=AXIS2_PLACEMENT_3D('',#22686,#17634,#17635);
#14131=AXIS2_PLACEMENT_3D('',#22688,#17636,#17637);
#14132=AXIS2_PLACEMENT_3D('',#22690,#17638,#17639);
#14133=AXIS2_PLACEMENT_3D('',#22692,#17640,#17641);
#14134=AXIS2_PLACEMENT_3D('',#22694,#17642,#17643);
#14135=AXIS2_PLACEMENT_3D('',#22696,#17644,#17645);
#14136=AXIS2_PLACEMENT_3D('',#22698,#17646,#17647);
#14137=AXIS2_PLACEMENT_3D('',#22700,#17648,#17649);
#14138=AXIS2_PLACEMENT_3D('',#22702,#17650,#17651);
#14139=AXIS2_PLACEMENT_3D('',#22704,#17652,#17653);
#14140=AXIS2_PLACEMENT_3D('',#22706,#17654,#17655);
#14141=AXIS2_PLACEMENT_3D('',#22708,#17656,#17657);
#14142=AXIS2_PLACEMENT_3D('',#22710,#17658,#17659);
#14143=AXIS2_PLACEMENT_3D('',#22712,#17660,#17661);
#14144=AXIS2_PLACEMENT_3D('',#22714,#17662,#17663);
#14145=AXIS2_PLACEMENT_3D('',#22716,#17664,#17665);
#14146=AXIS2_PLACEMENT_3D('',#22718,#17666,#17667);
#14147=AXIS2_PLACEMENT_3D('',#22720,#17668,#17669);
#14148=AXIS2_PLACEMENT_3D('',#22722,#17670,#17671);
#14149=AXIS2_PLACEMENT_3D('',#22724,#17672,#17673);
#14150=AXIS2_PLACEMENT_3D('',#22726,#17674,#17675);
#14151=AXIS2_PLACEMENT_3D('',#22728,#17676,#17677);
#14152=AXIS2_PLACEMENT_3D('',#22730,#17678,#17679);
#14153=AXIS2_PLACEMENT_3D('',#22732,#17680,#17681);
#14154=AXIS2_PLACEMENT_3D('',#22734,#17682,#17683);
#14155=AXIS2_PLACEMENT_3D('',#22736,#17684,#17685);
#14156=AXIS2_PLACEMENT_3D('',#22738,#17686,#17687);
#14157=AXIS2_PLACEMENT_3D('',#22740,#17688,#17689);
#14158=AXIS2_PLACEMENT_3D('',#22742,#17690,#17691);
#14159=AXIS2_PLACEMENT_3D('',#22744,#17692,#17693);
#14160=AXIS2_PLACEMENT_3D('',#22746,#17694,#17695);
#14161=AXIS2_PLACEMENT_3D('',#22748,#17696,#17697);
#14162=AXIS2_PLACEMENT_3D('',#22750,#17698,#17699);
#14163=AXIS2_PLACEMENT_3D('',#22752,#17700,#17701);
#14164=AXIS2_PLACEMENT_3D('',#22753,#17702,#17703);
#14165=AXIS2_PLACEMENT_3D('',#22754,#17704,#17705);
#14166=AXIS2_PLACEMENT_3D('',#22756,#17706,#17707);
#14167=AXIS2_PLACEMENT_3D('',#22758,#17709,#17710);
#14168=AXIS2_PLACEMENT_3D('',#22759,#17711,#17712);
#14169=AXIS2_PLACEMENT_3D('',#22761,#17713,#17714);
#14170=AXIS2_PLACEMENT_3D('',#22764,#17715,#17716);
#14171=AXIS2_PLACEMENT_3D('',#22766,#17717,#17718);
#14172=AXIS2_PLACEMENT_3D('',#22768,#17719,#17720);
#14173=AXIS2_PLACEMENT_3D('',#22770,#17721,#17722);
#14174=AXIS2_PLACEMENT_3D('',#22772,#17723,#17724);
#14175=AXIS2_PLACEMENT_3D('',#22774,#17725,#17726);
#14176=AXIS2_PLACEMENT_3D('',#22776,#17727,#17728);
#14177=AXIS2_PLACEMENT_3D('',#22778,#17729,#17730);
#14178=AXIS2_PLACEMENT_3D('',#22780,#17731,#17732);
#14179=AXIS2_PLACEMENT_3D('',#22782,#17733,#17734);
#14180=AXIS2_PLACEMENT_3D('',#22784,#17735,#17736);
#14181=AXIS2_PLACEMENT_3D('',#22786,#17737,#17738);
#14182=AXIS2_PLACEMENT_3D('',#22788,#17739,#17740);
#14183=AXIS2_PLACEMENT_3D('',#22790,#17741,#17742);
#14184=AXIS2_PLACEMENT_3D('',#22792,#17743,#17744);
#14185=AXIS2_PLACEMENT_3D('',#22794,#17745,#17746);
#14186=AXIS2_PLACEMENT_3D('',#22796,#17747,#17748);
#14187=AXIS2_PLACEMENT_3D('',#22798,#17749,#17750);
#14188=AXIS2_PLACEMENT_3D('',#22800,#17751,#17752);
#14189=AXIS2_PLACEMENT_3D('',#22802,#17753,#17754);
#14190=AXIS2_PLACEMENT_3D('',#22804,#17755,#17756);
#14191=AXIS2_PLACEMENT_3D('',#22806,#17757,#17758);
#14192=AXIS2_PLACEMENT_3D('',#22808,#17759,#17760);
#14193=AXIS2_PLACEMENT_3D('',#22810,#17761,#17762);
#14194=AXIS2_PLACEMENT_3D('',#22812,#17763,#17764);
#14195=AXIS2_PLACEMENT_3D('',#22814,#17765,#17766);
#14196=AXIS2_PLACEMENT_3D('',#22816,#17767,#17768);
#14197=AXIS2_PLACEMENT_3D('',#22818,#17769,#17770);
#14198=AXIS2_PLACEMENT_3D('',#22820,#17771,#17772);
#14199=AXIS2_PLACEMENT_3D('',#22822,#17773,#17774);
#14200=AXIS2_PLACEMENT_3D('',#22824,#17775,#17776);
#14201=AXIS2_PLACEMENT_3D('',#22826,#17777,#17778);
#14202=AXIS2_PLACEMENT_3D('',#22828,#17779,#17780);
#14203=AXIS2_PLACEMENT_3D('',#22830,#17781,#17782);
#14204=AXIS2_PLACEMENT_3D('',#22832,#17783,#17784);
#14205=AXIS2_PLACEMENT_3D('',#22834,#17785,#17786);
#14206=AXIS2_PLACEMENT_3D('',#22836,#17787,#17788);
#14207=AXIS2_PLACEMENT_3D('',#22838,#17789,#17790);
#14208=AXIS2_PLACEMENT_3D('',#22840,#17791,#17792);
#14209=AXIS2_PLACEMENT_3D('',#22842,#17793,#17794);
#14210=AXIS2_PLACEMENT_3D('',#22844,#17795,#17796);
#14211=AXIS2_PLACEMENT_3D('',#22846,#17797,#17798);
#14212=AXIS2_PLACEMENT_3D('',#22848,#17799,#17800);
#14213=AXIS2_PLACEMENT_3D('',#22850,#17801,#17802);
#14214=AXIS2_PLACEMENT_3D('',#22852,#17803,#17804);
#14215=AXIS2_PLACEMENT_3D('',#22854,#17805,#17806);
#14216=AXIS2_PLACEMENT_3D('',#22856,#17807,#17808);
#14217=AXIS2_PLACEMENT_3D('',#22858,#17809,#17810);
#14218=AXIS2_PLACEMENT_3D('',#22860,#17811,#17812);
#14219=AXIS2_PLACEMENT_3D('',#22862,#17813,#17814);
#14220=AXIS2_PLACEMENT_3D('',#22864,#17815,#17816);
#14221=AXIS2_PLACEMENT_3D('',#22866,#17817,#17818);
#14222=AXIS2_PLACEMENT_3D('',#22868,#17819,#17820);
#14223=AXIS2_PLACEMENT_3D('',#22870,#17821,#17822);
#14224=AXIS2_PLACEMENT_3D('',#22872,#17823,#17824);
#14225=AXIS2_PLACEMENT_3D('',#22874,#17825,#17826);
#14226=AXIS2_PLACEMENT_3D('',#22876,#17827,#17828);
#14227=AXIS2_PLACEMENT_3D('',#22878,#17829,#17830);
#14228=AXIS2_PLACEMENT_3D('',#22880,#17831,#17832);
#14229=AXIS2_PLACEMENT_3D('',#22882,#17833,#17834);
#14230=AXIS2_PLACEMENT_3D('',#22884,#17835,#17836);
#14231=AXIS2_PLACEMENT_3D('',#22886,#17837,#17838);
#14232=AXIS2_PLACEMENT_3D('',#22888,#17839,#17840);
#14233=AXIS2_PLACEMENT_3D('',#22890,#17841,#17842);
#14234=AXIS2_PLACEMENT_3D('',#22892,#17843,#17844);
#14235=AXIS2_PLACEMENT_3D('',#22894,#17845,#17846);
#14236=AXIS2_PLACEMENT_3D('',#22896,#17847,#17848);
#14237=AXIS2_PLACEMENT_3D('',#22898,#17849,#17850);
#14238=AXIS2_PLACEMENT_3D('',#22900,#17851,#17852);
#14239=AXIS2_PLACEMENT_3D('',#22902,#17853,#17854);
#14240=AXIS2_PLACEMENT_3D('',#22904,#17855,#17856);
#14241=AXIS2_PLACEMENT_3D('',#22906,#17857,#17858);
#14242=AXIS2_PLACEMENT_3D('',#22908,#17859,#17860);
#14243=AXIS2_PLACEMENT_3D('',#22910,#17861,#17862);
#14244=AXIS2_PLACEMENT_3D('',#22912,#17863,#17864);
#14245=AXIS2_PLACEMENT_3D('',#22914,#17865,#17866);
#14246=AXIS2_PLACEMENT_3D('',#22916,#17867,#17868);
#14247=AXIS2_PLACEMENT_3D('',#22918,#17869,#17870);
#14248=AXIS2_PLACEMENT_3D('',#22920,#17871,#17872);
#14249=AXIS2_PLACEMENT_3D('',#22921,#17873,#17874);
#14250=AXIS2_PLACEMENT_3D('',#22922,#17875,#17876);
#14251=AXIS2_PLACEMENT_3D('',#22924,#17877,#17878);
#14252=AXIS2_PLACEMENT_3D('',#22926,#17880,#17881);
#14253=AXIS2_PLACEMENT_3D('',#22927,#17882,#17883);
#14254=AXIS2_PLACEMENT_3D('',#22930,#17886,#17887);
#14255=AXIS2_PLACEMENT_3D('',#22932,#17889,#17890);
#14256=AXIS2_PLACEMENT_3D('',#22934,#17892,#17893);
#14257=AXIS2_PLACEMENT_3D('',#22936,#17895,#17896);
#14258=AXIS2_PLACEMENT_3D('',#22938,#17898,#17899);
#14259=AXIS2_PLACEMENT_3D('',#22940,#17901,#17902);
#14260=AXIS2_PLACEMENT_3D('',#22942,#17904,#17905);
#14261=AXIS2_PLACEMENT_3D('',#22944,#17907,#17908);
#14262=AXIS2_PLACEMENT_3D('',#22946,#17910,#17911);
#14263=AXIS2_PLACEMENT_3D('',#22948,#17913,#17914);
#14264=AXIS2_PLACEMENT_3D('',#22950,#17916,#17917);
#14265=AXIS2_PLACEMENT_3D('',#22952,#17919,#17920);
#14266=AXIS2_PLACEMENT_3D('',#22954,#17922,#17923);
#14267=AXIS2_PLACEMENT_3D('',#22956,#17925,#17926);
#14268=AXIS2_PLACEMENT_3D('',#22958,#17928,#17929);
#14269=AXIS2_PLACEMENT_3D('',#22960,#17931,#17932);
#14270=AXIS2_PLACEMENT_3D('',#22962,#17934,#17935);
#14271=AXIS2_PLACEMENT_3D('',#22964,#17937,#17938);
#14272=AXIS2_PLACEMENT_3D('',#22966,#17940,#17941);
#14273=AXIS2_PLACEMENT_3D('',#22968,#17943,#17944);
#14274=AXIS2_PLACEMENT_3D('',#22970,#17946,#17947);
#14275=AXIS2_PLACEMENT_3D('',#22972,#17949,#17950);
#14276=AXIS2_PLACEMENT_3D('',#22974,#17952,#17953);
#14277=AXIS2_PLACEMENT_3D('',#22976,#17955,#17956);
#14278=AXIS2_PLACEMENT_3D('',#22978,#17958,#17959);
#14279=AXIS2_PLACEMENT_3D('',#22980,#17961,#17962);
#14280=AXIS2_PLACEMENT_3D('',#22982,#17964,#17965);
#14281=AXIS2_PLACEMENT_3D('',#22984,#17967,#17968);
#14282=AXIS2_PLACEMENT_3D('',#22986,#17970,#17971);
#14283=AXIS2_PLACEMENT_3D('',#22988,#17973,#17974);
#14284=AXIS2_PLACEMENT_3D('',#22990,#17976,#17977);
#14285=AXIS2_PLACEMENT_3D('',#22992,#17979,#17980);
#14286=AXIS2_PLACEMENT_3D('',#22994,#17982,#17983);
#14287=AXIS2_PLACEMENT_3D('',#22996,#17985,#17986);
#14288=AXIS2_PLACEMENT_3D('',#22998,#17988,#17989);
#14289=AXIS2_PLACEMENT_3D('',#23000,#17991,#17992);
#14290=AXIS2_PLACEMENT_3D('',#23002,#17994,#17995);
#14291=AXIS2_PLACEMENT_3D('',#23004,#17997,#17998);
#14292=AXIS2_PLACEMENT_3D('',#23006,#18000,#18001);
#14293=AXIS2_PLACEMENT_3D('',#23008,#18003,#18004);
#14294=AXIS2_PLACEMENT_3D('',#23010,#18006,#18007);
#14295=AXIS2_PLACEMENT_3D('',#23012,#18009,#18010);
#14296=AXIS2_PLACEMENT_3D('',#23014,#18012,#18013);
#14297=AXIS2_PLACEMENT_3D('',#23016,#18015,#18016);
#14298=AXIS2_PLACEMENT_3D('',#23018,#18018,#18019);
#14299=AXIS2_PLACEMENT_3D('',#23020,#18021,#18022);
#14300=AXIS2_PLACEMENT_3D('',#23022,#18024,#18025);
#14301=AXIS2_PLACEMENT_3D('',#23024,#18027,#18028);
#14302=AXIS2_PLACEMENT_3D('',#23026,#18030,#18031);
#14303=AXIS2_PLACEMENT_3D('',#23028,#18033,#18034);
#14304=AXIS2_PLACEMENT_3D('',#23030,#18036,#18037);
#14305=AXIS2_PLACEMENT_3D('',#23032,#18039,#18040);
#14306=AXIS2_PLACEMENT_3D('',#23034,#18042,#18043);
#14307=AXIS2_PLACEMENT_3D('',#23036,#18045,#18046);
#14308=AXIS2_PLACEMENT_3D('',#23038,#18048,#18049);
#14309=AXIS2_PLACEMENT_3D('',#23040,#18051,#18052);
#14310=AXIS2_PLACEMENT_3D('',#23042,#18054,#18055);
#14311=AXIS2_PLACEMENT_3D('',#23044,#18057,#18058);
#14312=AXIS2_PLACEMENT_3D('',#23046,#18060,#18061);
#14313=AXIS2_PLACEMENT_3D('',#23048,#18063,#18064);
#14314=AXIS2_PLACEMENT_3D('',#23050,#18066,#18067);
#14315=AXIS2_PLACEMENT_3D('',#23052,#18069,#18070);
#14316=AXIS2_PLACEMENT_3D('',#23054,#18072,#18073);
#14317=AXIS2_PLACEMENT_3D('',#23056,#18075,#18076);
#14318=AXIS2_PLACEMENT_3D('',#23058,#18078,#18079);
#14319=AXIS2_PLACEMENT_3D('',#23060,#18081,#18082);
#14320=AXIS2_PLACEMENT_3D('',#23062,#18084,#18085);
#14321=AXIS2_PLACEMENT_3D('',#23064,#18087,#18088);
#14322=AXIS2_PLACEMENT_3D('',#23066,#18090,#18091);
#14323=AXIS2_PLACEMENT_3D('',#23068,#18093,#18094);
#14324=AXIS2_PLACEMENT_3D('',#23070,#18096,#18097);
#14325=AXIS2_PLACEMENT_3D('',#23072,#18099,#18100);
#14326=AXIS2_PLACEMENT_3D('',#23074,#18102,#18103);
#14327=AXIS2_PLACEMENT_3D('',#23076,#18105,#18106);
#14328=AXIS2_PLACEMENT_3D('',#23078,#18108,#18109);
#14329=AXIS2_PLACEMENT_3D('',#23080,#18111,#18112);
#14330=AXIS2_PLACEMENT_3D('',#23082,#18114,#18115);
#14331=AXIS2_PLACEMENT_3D('',#23084,#18117,#18118);
#14332=AXIS2_PLACEMENT_3D('',#23086,#18120,#18121);
#14333=AXIS2_PLACEMENT_3D('',#23087,#18122,#18123);
#14334=AXIS2_PLACEMENT_3D('',#23088,#18124,#18125);
#14335=AXIS2_PLACEMENT_3D('',#23090,#18126,#18127);
#14336=AXIS2_PLACEMENT_3D('',#23091,#18128,#18129);
#14337=AXIS2_PLACEMENT_3D('',#23093,#18130,#18131);
#14338=AXIS2_PLACEMENT_3D('',#23095,#18133,#18134);
#14339=AXIS2_PLACEMENT_3D('',#23097,#18135,#18136);
#14340=AXIS2_PLACEMENT_3D('',#23099,#18138,#18139);
#14341=AXIS2_PLACEMENT_3D('',#23101,#18140,#18141);
#14342=AXIS2_PLACEMENT_3D('',#23103,#18143,#18144);
#14343=AXIS2_PLACEMENT_3D('',#23105,#18145,#18146);
#14344=AXIS2_PLACEMENT_3D('',#23106,#18147,#18148);
#14345=AXIS2_PLACEMENT_3D('',#23108,#18149,#18150);
#14346=AXIS2_PLACEMENT_3D('',#23110,#18152,#18153);
#14347=AXIS2_PLACEMENT_3D('',#23112,#18154,#18155);
#14348=AXIS2_PLACEMENT_3D('',#23114,#18157,#18158);
#14349=AXIS2_PLACEMENT_3D('',#23116,#18159,#18160);
#14350=AXIS2_PLACEMENT_3D('',#23118,#18162,#18163);
#14351=AXIS2_PLACEMENT_3D('',#23119,#18164,#18165);
#14352=AXIS2_PLACEMENT_3D('',#23128,#18170,#18171);
#14353=AXIS2_PLACEMENT_3D('',#23134,#18175,#18176);
#14354=AXIS2_PLACEMENT_3D('',#23140,#18180,#18181);
#14355=AXIS2_PLACEMENT_3D('',#23146,#18185,#18186);
#14356=AXIS2_PLACEMENT_3D('',#23152,#18190,#18191);
#14357=AXIS2_PLACEMENT_3D('',#23155,#18194,#18195);
#14358=AXIS2_PLACEMENT_3D('',#23156,#18196,#18197);
#14359=AXIS2_PLACEMENT_3D('',#23157,#18198,#18199);
#14360=AXIS2_PLACEMENT_3D('',#23158,#18200,#18201);
#14361=AXIS2_PLACEMENT_3D('',#23159,#18202,#18203);
#14362=AXIS2_PLACEMENT_3D('',#23160,#18204,#18205);
#14363=AXIS2_PLACEMENT_3D('',#23161,#18206,#18207);
#14364=AXIS2_PLACEMENT_3D('',#23162,#18208,#18209);
#14365=AXIS2_PLACEMENT_3D('',#23163,#18210,#18211);
#14366=AXIS2_PLACEMENT_3D('',#23164,#18212,#18213);
#14367=AXIS2_PLACEMENT_3D('',#23165,#18214,#18215);
#14368=AXIS2_PLACEMENT_3D('',#23166,#18216,#18217);
#14369=AXIS2_PLACEMENT_3D('',#23167,#18218,#18219);
#14370=AXIS2_PLACEMENT_3D('',#23168,#18220,#18221);
#14371=AXIS2_PLACEMENT_3D('',#23169,#18222,#18223);
#14372=AXIS2_PLACEMENT_3D('',#23170,#18224,#18225);
#14373=AXIS2_PLACEMENT_3D('',#23171,#18226,#18227);
#14374=AXIS2_PLACEMENT_3D('',#23172,#18228,#18229);
#14375=AXIS2_PLACEMENT_3D('',#23173,#18230,#18231);
#14376=AXIS2_PLACEMENT_3D('',#23174,#18232,#18233);
#14377=AXIS2_PLACEMENT_3D('',#23175,#18234,#18235);
#14378=AXIS2_PLACEMENT_3D('',#23176,#18236,#18237);
#14379=AXIS2_PLACEMENT_3D('',#23177,#18238,#18239);
#14380=AXIS2_PLACEMENT_3D('',#23178,#18240,#18241);
#14381=AXIS2_PLACEMENT_3D('',#23179,#18242,#18243);
#14382=AXIS2_PLACEMENT_3D('',#23180,#18244,#18245);
#14383=AXIS2_PLACEMENT_3D('',#23181,#18246,#18247);
#14384=AXIS2_PLACEMENT_3D('',#23182,#18248,#18249);
#14385=AXIS2_PLACEMENT_3D('',#23183,#18250,#18251);
#14386=AXIS2_PLACEMENT_3D('',#23184,#18252,#18253);
#14387=AXIS2_PLACEMENT_3D('',#23185,#18254,#18255);
#14388=AXIS2_PLACEMENT_3D('',#23186,#18256,#18257);
#14389=AXIS2_PLACEMENT_3D('',#23187,#18258,#18259);
#14390=AXIS2_PLACEMENT_3D('',#23188,#18260,#18261);
#14391=AXIS2_PLACEMENT_3D('',#23189,#18262,#18263);
#14392=AXIS2_PLACEMENT_3D('',#23190,#18264,#18265);
#14393=AXIS2_PLACEMENT_3D('',#23191,#18266,#18267);
#14394=AXIS2_PLACEMENT_3D('',#23192,#18268,#18269);
#14395=AXIS2_PLACEMENT_3D('',#23193,#18270,#18271);
#14396=AXIS2_PLACEMENT_3D('',#23194,#18272,#18273);
#14397=AXIS2_PLACEMENT_3D('',#23195,#18274,#18275);
#14398=AXIS2_PLACEMENT_3D('',#23196,#18276,#18277);
#14399=AXIS2_PLACEMENT_3D('',#23197,#18278,#18279);
#14400=AXIS2_PLACEMENT_3D('',#23198,#18280,#18281);
#14401=AXIS2_PLACEMENT_3D('',#23199,#18282,#18283);
#14402=AXIS2_PLACEMENT_3D('',#23200,#18284,#18285);
#14403=AXIS2_PLACEMENT_3D('',#23201,#18286,#18287);
#14404=AXIS2_PLACEMENT_3D('',#23202,#18288,#18289);
#14405=AXIS2_PLACEMENT_3D('',#23203,#18290,#18291);
#14406=AXIS2_PLACEMENT_3D('',#23204,#18292,#18293);
#14407=AXIS2_PLACEMENT_3D('',#23205,#18294,#18295);
#14408=AXIS2_PLACEMENT_3D('',#23206,#18296,#18297);
#14409=AXIS2_PLACEMENT_3D('',#23207,#18298,#18299);
#14410=AXIS2_PLACEMENT_3D('',#23208,#18300,#18301);
#14411=AXIS2_PLACEMENT_3D('',#23209,#18302,#18303);
#14412=AXIS2_PLACEMENT_3D('',#23210,#18304,#18305);
#14413=AXIS2_PLACEMENT_3D('',#23211,#18306,#18307);
#14414=AXIS2_PLACEMENT_3D('',#23212,#18308,#18309);
#14415=AXIS2_PLACEMENT_3D('',#23213,#18310,#18311);
#14416=AXIS2_PLACEMENT_3D('',#23215,#18312,#18313);
#14417=AXIS2_PLACEMENT_3D('',#23218,#18315,#18316);
#14418=AXIS2_PLACEMENT_3D('',#23219,#18317,#18318);
#14419=AXIS2_PLACEMENT_3D('',#23220,#18319,#18320);
#14420=AXIS2_PLACEMENT_3D('',#23222,#18321,#18322);
#14421=AXIS2_PLACEMENT_3D('',#23224,#18323,#18324);
#14422=AXIS2_PLACEMENT_3D('',#23225,#18325,#18326);
#14423=AXIS2_PLACEMENT_3D('',#23227,#18327,#18328);
#14424=AXIS2_PLACEMENT_3D('',#23229,#18329,#18330);
#14425=AXIS2_PLACEMENT_3D('',#23230,#18331,#18332);
#14426=AXIS2_PLACEMENT_3D('',#23232,#18334,#18335);
#14427=AXIS2_PLACEMENT_3D('',#23235,#18337,#18338);
#14428=AXIS2_PLACEMENT_3D('',#23236,#18339,#18340);
#14429=AXIS2_PLACEMENT_3D('',#23238,#18341,#18342);
#14430=AXIS2_PLACEMENT_3D('',#23240,#18343,#18344);
#14431=AXIS2_PLACEMENT_3D('',#23241,#18345,#18346);
#14432=AXIS2_PLACEMENT_3D('',#23243,#18347,#18348);
#14433=AXIS2_PLACEMENT_3D('',#23245,#18349,#18350);
#14434=AXIS2_PLACEMENT_3D('',#23246,#18351,#18352);
#14435=AXIS2_PLACEMENT_3D('',#23248,#18354,#18355);
#14436=AXIS2_PLACEMENT_3D('',#23251,#18357,#18358);
#14437=AXIS2_PLACEMENT_3D('',#23252,#18359,#18360);
#14438=AXIS2_PLACEMENT_3D('',#23254,#18361,#18362);
#14439=AXIS2_PLACEMENT_3D('',#23255,#18363,#18364);
#14440=AXIS2_PLACEMENT_3D('',#23257,#18365,#18366);
#14441=AXIS2_PLACEMENT_3D('',#23259,#18368,#18369);
#14442=AXIS2_PLACEMENT_3D('',#23261,#18370,#18371);
#14443=AXIS2_PLACEMENT_3D('',#23263,#18372,#18373);
#14444=AXIS2_PLACEMENT_3D('',#23264,#18374,#18375);
#14445=AXIS2_PLACEMENT_3D('',#23266,#18377,#18378);
#14446=AXIS2_PLACEMENT_3D('',#23268,#18380,#18381);
#14447=AXIS2_PLACEMENT_3D('',#23269,#18382,#18383);
#14448=AXIS2_PLACEMENT_3D('',#23270,#18384,#18385);
#14449=AXIS2_PLACEMENT_3D('',#23271,#18386,#18387);
#14450=AXIS2_PLACEMENT_3D('',#23275,#18389,#18390);
#14451=AXIS2_PLACEMENT_3D('',#23276,#18391,#18392);
#14452=AXIS2_PLACEMENT_3D('',#23286,#18393,#18394);
#14453=AXIS2_PLACEMENT_3D('',#23348,#18396,#18397);
#14454=AXIS2_PLACEMENT_3D('',#23350,#18399,#18400);
#14455=AXIS2_PLACEMENT_3D('',#23352,#18401,#18402);
#14456=AXIS2_PLACEMENT_3D('',#23356,#18405,#18406);
#14457=AXIS2_PLACEMENT_3D('',#23357,#18407,#18408);
#14458=AXIS2_PLACEMENT_3D('',#23359,#18409,#18410);
#14459=AXIS2_PLACEMENT_3D('',#23363,#18413,#18414);
#14460=AXIS2_PLACEMENT_3D('',#23364,#18415,#18416);
#14461=AXIS2_PLACEMENT_3D('',#23365,#18417,#18418);
#14462=AXIS2_PLACEMENT_3D('',#23366,#18419,#18420);
#14463=AXIS2_PLACEMENT_3D('',#23367,#18421,#18422);
#14464=AXIS2_PLACEMENT_3D('',#23376,#18427,#18428);
#14465=AXIS2_PLACEMENT_3D('',#23382,#18432,#18433);
#14466=AXIS2_PLACEMENT_3D('',#23388,#18437,#18438);
#14467=AXIS2_PLACEMENT_3D('',#23394,#18442,#18443);
#14468=AXIS2_PLACEMENT_3D('',#23400,#18447,#18448);
#14469=AXIS2_PLACEMENT_3D('',#23403,#18451,#18452);
#14470=AXIS2_PLACEMENT_3D('',#23404,#18453,#18454);
#14471=AXIS2_PLACEMENT_3D('',#23406,#18455,#18456);
#14472=AXIS2_PLACEMENT_3D('',#23407,#18457,#18458);
#14473=AXIS2_PLACEMENT_3D('',#23409,#18459,#18460);
#14474=AXIS2_PLACEMENT_3D('',#23411,#18462,#18463);
#14475=AXIS2_PLACEMENT_3D('',#23413,#18464,#18465);
#14476=AXIS2_PLACEMENT_3D('',#23415,#18467,#18468);
#14477=AXIS2_PLACEMENT_3D('',#23417,#18469,#18470);
#14478=AXIS2_PLACEMENT_3D('',#23419,#18472,#18473);
#14479=AXIS2_PLACEMENT_3D('',#23420,#18474,#18475);
#14480=AXIS2_PLACEMENT_3D('',#23421,#18476,#18477);
#14481=AXIS2_PLACEMENT_3D('',#23422,#18478,#18479);
#14482=AXIS2_PLACEMENT_3D('',#23423,#18480,#18481);
#14483=AXIS2_PLACEMENT_3D('',#23424,#18482,#18483);
#14484=AXIS2_PLACEMENT_3D('',#23425,#18484,#18485);
#14485=AXIS2_PLACEMENT_3D('',#23426,#18486,#18487);
#14486=AXIS2_PLACEMENT_3D('',#23427,#18488,#18489);
#14487=AXIS2_PLACEMENT_3D('',#23428,#18490,#18491);
#14488=AXIS2_PLACEMENT_3D('',#23429,#18492,#18493);
#14489=AXIS2_PLACEMENT_3D('',#23430,#18494,#18495);
#14490=AXIS2_PLACEMENT_3D('',#23431,#18496,#18497);
#14491=AXIS2_PLACEMENT_3D('',#23432,#18498,#18499);
#14492=AXIS2_PLACEMENT_3D('',#23433,#18500,#18501);
#14493=AXIS2_PLACEMENT_3D('',#23434,#18502,#18503);
#14494=AXIS2_PLACEMENT_3D('',#23435,#18504,#18505);
#14495=AXIS2_PLACEMENT_3D('',#23436,#18506,#18507);
#14496=AXIS2_PLACEMENT_3D('',#23437,#18508,#18509);
#14497=AXIS2_PLACEMENT_3D('',#23438,#18510,#18511);
#14498=AXIS2_PLACEMENT_3D('',#23439,#18512,#18513);
#14499=AXIS2_PLACEMENT_3D('',#23440,#18514,#18515);
#14500=AXIS2_PLACEMENT_3D('',#23441,#18516,#18517);
#14501=AXIS2_PLACEMENT_3D('',#23442,#18518,#18519);
#14502=AXIS2_PLACEMENT_3D('',#23443,#18520,#18521);
#14503=AXIS2_PLACEMENT_3D('',#23444,#18522,#18523);
#14504=AXIS2_PLACEMENT_3D('',#23445,#18524,#18525);
#14505=AXIS2_PLACEMENT_3D('',#23446,#18526,#18527);
#14506=AXIS2_PLACEMENT_3D('',#23447,#18528,#18529);
#14507=AXIS2_PLACEMENT_3D('',#23448,#18530,#18531);
#14508=AXIS2_PLACEMENT_3D('',#23449,#18532,#18533);
#14509=AXIS2_PLACEMENT_3D('',#23450,#18534,#18535);
#14510=AXIS2_PLACEMENT_3D('',#23451,#18536,#18537);
#14511=AXIS2_PLACEMENT_3D('',#23452,#18538,#18539);
#14512=AXIS2_PLACEMENT_3D('',#23453,#18540,#18541);
#14513=AXIS2_PLACEMENT_3D('',#23454,#18542,#18543);
#14514=AXIS2_PLACEMENT_3D('',#23455,#18544,#18545);
#14515=AXIS2_PLACEMENT_3D('',#23456,#18546,#18547);
#14516=AXIS2_PLACEMENT_3D('',#23457,#18548,#18549);
#14517=DIRECTION('axis',(0.,0.,1.));
#14518=DIRECTION('refdir',(1.,0.,0.));
#14519=DIRECTION('axis',(0.,0.,1.));
#14520=DIRECTION('refdir',(1.,0.,0.));
#14521=DIRECTION('axis',(0.,0.,1.));
#14522=DIRECTION('refdir',(1.,0.,0.));
#14523=DIRECTION('center_axis',(0.,0.,1.));
#14524=DIRECTION('ref_axis',(1.,0.,0.));
#14525=DIRECTION('center_axis',(0.,0.,1.));
#14526=DIRECTION('ref_axis',(1.,0.,0.));
#14527=DIRECTION('',(0.,0.,1.));
#14528=DIRECTION('center_axis',(0.,0.,-1.));
#14529=DIRECTION('ref_axis',(1.,0.,0.));
#14530=DIRECTION('center_axis',(0.,0.,1.));
#14531=DIRECTION('ref_axis',(1.,0.,0.));
#14532=DIRECTION('center_axis',(0.,0.,1.));
#14533=DIRECTION('ref_axis',(1.,0.,0.));
#14534=DIRECTION('center_axis',(0.,0.,1.));
#14535=DIRECTION('ref_axis',(1.,0.,0.));
#14536=DIRECTION('',(0.,0.,1.));
#14537=DIRECTION('center_axis',(0.,0.,-1.));
#14538=DIRECTION('ref_axis',(1.,0.,0.));
#14539=DIRECTION('center_axis',(0.,0.,1.));
#14540=DIRECTION('ref_axis',(1.,0.,0.));
#14541=DIRECTION('center_axis',(0.,0.,1.));
#14542=DIRECTION('ref_axis',(1.,0.,0.));
#14543=DIRECTION('center_axis',(0.,0.,1.));
#14544=DIRECTION('ref_axis',(1.,0.,0.));
#14545=DIRECTION('',(0.,0.,1.));
#14546=DIRECTION('center_axis',(0.,0.,-1.));
#14547=DIRECTION('ref_axis',(1.,0.,0.));
#14548=DIRECTION('center_axis',(0.,0.,1.));
#14549=DIRECTION('ref_axis',(1.,0.,0.));
#14550=DIRECTION('center_axis',(0.,0.,1.));
#14551=DIRECTION('ref_axis',(1.,0.,0.));
#14552=DIRECTION('center_axis',(0.,0.,1.));
#14553=DIRECTION('ref_axis',(1.,0.,0.));
#14554=DIRECTION('',(0.,0.,1.));
#14555=DIRECTION('center_axis',(0.,0.,-1.));
#14556=DIRECTION('ref_axis',(1.,0.,0.));
#14557=DIRECTION('center_axis',(0.,0.,1.));
#14558=DIRECTION('ref_axis',(1.,0.,0.));
#14559=DIRECTION('center_axis',(0.,0.,1.));
#14560=DIRECTION('ref_axis',(1.,0.,0.));
#14561=DIRECTION('center_axis',(0.,0.,1.));
#14562=DIRECTION('ref_axis',(1.,0.,0.));
#14563=DIRECTION('',(0.,0.,1.));
#14564=DIRECTION('center_axis',(0.,0.,-1.));
#14565=DIRECTION('ref_axis',(1.,0.,0.));
#14566=DIRECTION('center_axis',(0.,0.,1.));
#14567=DIRECTION('ref_axis',(1.,0.,0.));
#14568=DIRECTION('center_axis',(0.,0.,1.));
#14569=DIRECTION('ref_axis',(1.,0.,0.));
#14570=DIRECTION('center_axis',(0.,0.,1.));
#14571=DIRECTION('ref_axis',(1.,0.,0.));
#14572=DIRECTION('',(0.,0.,1.));
#14573=DIRECTION('center_axis',(0.,0.,-1.));
#14574=DIRECTION('ref_axis',(1.,0.,0.));
#14575=DIRECTION('center_axis',(0.,0.,1.));
#14576=DIRECTION('ref_axis',(1.,0.,0.));
#14577=DIRECTION('center_axis',(0.,0.,1.));
#14578=DIRECTION('ref_axis',(1.,0.,0.));
#14579=DIRECTION('center_axis',(0.,0.,1.));
#14580=DIRECTION('ref_axis',(1.,0.,0.));
#14581=DIRECTION('',(0.,0.,1.));
#14582=DIRECTION('center_axis',(0.,0.,-1.));
#14583=DIRECTION('ref_axis',(1.,0.,0.));
#14584=DIRECTION('center_axis',(0.,0.,1.));
#14585=DIRECTION('ref_axis',(1.,0.,0.));
#14586=DIRECTION('center_axis',(0.,0.,1.));
#14587=DIRECTION('ref_axis',(1.,0.,0.));
#14588=DIRECTION('center_axis',(0.,0.,1.));
#14589=DIRECTION('ref_axis',(1.,0.,0.));
#14590=DIRECTION('',(0.,0.,1.));
#14591=DIRECTION('center_axis',(0.,0.,-1.));
#14592=DIRECTION('ref_axis',(1.,0.,0.));
#14593=DIRECTION('center_axis',(0.,0.,1.));
#14594=DIRECTION('ref_axis',(1.,0.,0.));
#14595=DIRECTION('center_axis',(0.,0.,1.));
#14596=DIRECTION('ref_axis',(1.,0.,0.));
#14597=DIRECTION('center_axis',(0.,0.,1.));
#14598=DIRECTION('ref_axis',(1.,0.,0.));
#14599=DIRECTION('',(0.,0.,1.));
#14600=DIRECTION('center_axis',(0.,0.,-1.));
#14601=DIRECTION('ref_axis',(1.,0.,0.));
#14602=DIRECTION('center_axis',(0.,0.,1.));
#14603=DIRECTION('ref_axis',(1.,0.,0.));
#14604=DIRECTION('center_axis',(0.,0.,1.));
#14605=DIRECTION('ref_axis',(1.,0.,0.));
#14606=DIRECTION('center_axis',(0.,0.,1.));
#14607=DIRECTION('ref_axis',(1.,0.,0.));
#14608=DIRECTION('',(0.,0.,1.));
#14609=DIRECTION('center_axis',(0.,0.,-1.));
#14610=DIRECTION('ref_axis',(1.,0.,0.));
#14611=DIRECTION('center_axis',(0.,0.,1.));
#14612=DIRECTION('ref_axis',(1.,0.,0.));
#14613=DIRECTION('center_axis',(0.,0.,1.));
#14614=DIRECTION('ref_axis',(1.,0.,0.));
#14615=DIRECTION('center_axis',(0.,0.,1.));
#14616=DIRECTION('ref_axis',(1.,0.,0.));
#14617=DIRECTION('',(0.,0.,1.));
#14618=DIRECTION('center_axis',(0.,0.,-1.));
#14619=DIRECTION('ref_axis',(1.,0.,0.));
#14620=DIRECTION('center_axis',(0.,0.,1.));
#14621=DIRECTION('ref_axis',(1.,0.,0.));
#14622=DIRECTION('center_axis',(0.,0.,1.));
#14623=DIRECTION('ref_axis',(1.,0.,0.));
#14624=DIRECTION('center_axis',(0.,0.,1.));
#14625=DIRECTION('ref_axis',(1.,0.,0.));
#14626=DIRECTION('',(0.,0.,1.));
#14627=DIRECTION('center_axis',(0.,0.,-1.));
#14628=DIRECTION('ref_axis',(1.,0.,0.));
#14629=DIRECTION('center_axis',(0.,0.,1.));
#14630=DIRECTION('ref_axis',(1.,0.,0.));
#14631=DIRECTION('center_axis',(0.,0.,1.));
#14632=DIRECTION('ref_axis',(1.,0.,0.));
#14633=DIRECTION('center_axis',(0.,0.,1.));
#14634=DIRECTION('ref_axis',(1.,0.,0.));
#14635=DIRECTION('',(0.,0.,1.));
#14636=DIRECTION('center_axis',(0.,0.,-1.));
#14637=DIRECTION('ref_axis',(1.,0.,0.));
#14638=DIRECTION('center_axis',(0.,0.,1.));
#14639=DIRECTION('ref_axis',(1.,0.,0.));
#14640=DIRECTION('center_axis',(0.,0.,1.));
#14641=DIRECTION('ref_axis',(1.,0.,0.));
#14642=DIRECTION('center_axis',(0.,0.,1.));
#14643=DIRECTION('ref_axis',(1.,0.,0.));
#14644=DIRECTION('',(0.,0.,1.));
#14645=DIRECTION('center_axis',(0.,0.,-1.));
#14646=DIRECTION('ref_axis',(1.,0.,0.));
#14647=DIRECTION('center_axis',(0.,0.,1.));
#14648=DIRECTION('ref_axis',(1.,0.,0.));
#14649=DIRECTION('center_axis',(0.,1.,0.));
#14650=DIRECTION('ref_axis',(-1.,0.,0.));
#14651=DIRECTION('',(-1.,0.,0.));
#14652=DIRECTION('',(0.,0.,1.));
#14653=DIRECTION('',(-1.,0.,0.));
#14654=DIRECTION('',(0.,0.,1.));
#14655=DIRECTION('center_axis',(1.,0.,0.));
#14656=DIRECTION('ref_axis',(0.,1.,0.));
#14657=DIRECTION('',(0.,1.,0.));
#14658=DIRECTION('',(0.,1.,0.));
#14659=DIRECTION('',(0.,0.,1.));
#14660=DIRECTION('center_axis',(0.,-1.,0.));
#14661=DIRECTION('ref_axis',(1.,0.,0.));
#14662=DIRECTION('',(1.,0.,0.));
#14663=DIRECTION('',(1.,0.,0.));
#14664=DIRECTION('',(0.,0.,1.));
#14665=DIRECTION('center_axis',(-1.,0.,0.));
#14666=DIRECTION('ref_axis',(0.,-1.,0.));
#14667=DIRECTION('',(0.,-1.,0.));
#14668=DIRECTION('',(0.,-1.,0.));
#14669=DIRECTION('center_axis',(0.,0.,1.));
#14670=DIRECTION('ref_axis',(1.,0.,0.));
#14671=DIRECTION('center_axis',(0.,0.,1.));
#14672=DIRECTION('ref_axis',(1.,0.,0.));
#14673=DIRECTION('axis',(0.,0.,1.));
#14674=DIRECTION('refdir',(1.,0.,0.));
#14675=DIRECTION('center_axis',(0.,1.,0.));
#14676=DIRECTION('ref_axis',(-1.,0.,0.));
#14677=DIRECTION('',(-1.,0.,0.));
#14678=DIRECTION('',(0.,0.,1.));
#14679=DIRECTION('',(-1.,0.,0.));
#14680=DIRECTION('',(0.,0.,1.));
#14681=DIRECTION('center_axis',(1.,0.,0.));
#14682=DIRECTION('ref_axis',(0.,1.,0.));
#14683=DIRECTION('',(0.,1.,0.));
#14684=DIRECTION('',(0.,1.,0.));
#14685=DIRECTION('',(0.,0.,1.));
#14686=DIRECTION('center_axis',(0.,-1.,0.));
#14687=DIRECTION('ref_axis',(1.,0.,0.));
#14688=DIRECTION('',(1.,0.,0.));
#14689=DIRECTION('',(1.,0.,0.));
#14690=DIRECTION('',(0.,0.,1.));
#14691=DIRECTION('center_axis',(-1.,0.,0.));
#14692=DIRECTION('ref_axis',(0.,-1.,0.));
#14693=DIRECTION('',(0.,-1.,0.));
#14694=DIRECTION('',(0.,-1.,0.));
#14695=DIRECTION('center_axis',(0.,0.,1.));
#14696=DIRECTION('ref_axis',(1.,0.,0.));
#14697=DIRECTION('center_axis',(0.,0.,1.));
#14698=DIRECTION('ref_axis',(1.,0.,0.));
#14699=DIRECTION('axis',(0.,0.,1.));
#14700=DIRECTION('refdir',(1.,0.,0.));
#14701=DIRECTION('center_axis',(0.,1.,0.));
#14702=DIRECTION('ref_axis',(-1.,0.,0.));
#14703=DIRECTION('',(-1.,0.,0.));
#14704=DIRECTION('',(0.,0.,1.));
#14705=DIRECTION('',(-1.,0.,0.));
#14706=DIRECTION('',(0.,0.,1.));
#14707=DIRECTION('center_axis',(1.,0.,0.));
#14708=DIRECTION('ref_axis',(0.,1.,0.));
#14709=DIRECTION('',(0.,1.,0.));
#14710=DIRECTION('',(0.,1.,0.));
#14711=DIRECTION('',(0.,0.,1.));
#14712=DIRECTION('center_axis',(0.,-1.,0.));
#14713=DIRECTION('ref_axis',(1.,0.,0.));
#14714=DIRECTION('',(1.,0.,0.));
#14715=DIRECTION('',(1.,0.,0.));
#14716=DIRECTION('',(0.,0.,1.));
#14717=DIRECTION('center_axis',(-1.,0.,0.));
#14718=DIRECTION('ref_axis',(0.,-1.,0.));
#14719=DIRECTION('',(0.,-1.,0.));
#14720=DIRECTION('',(0.,-1.,0.));
#14721=DIRECTION('center_axis',(0.,0.,1.));
#14722=DIRECTION('ref_axis',(1.,0.,0.));
#14723=DIRECTION('center_axis',(0.,0.,1.));
#14724=DIRECTION('ref_axis',(1.,0.,0.));
#14725=DIRECTION('axis',(0.,0.,1.));
#14726=DIRECTION('refdir',(1.,0.,0.));
#14727=DIRECTION('center_axis',(0.,1.,0.));
#14728=DIRECTION('ref_axis',(1.,0.,0.));
#14729=DIRECTION('center_axis',(0.,1.,0.));
#14730=DIRECTION('ref_axis',(1.,0.,0.));
#14731=DIRECTION('',(0.,1.,0.));
#14732=DIRECTION('center_axis',(0.,-1.,0.));
#14733=DIRECTION('ref_axis',(1.,0.,0.));
#14734=DIRECTION('center_axis',(0.,1.,0.));
#14735=DIRECTION('ref_axis',(1.,0.,0.));
#14736=DIRECTION('center_axis',(0.,1.,0.));
#14737=DIRECTION('ref_axis',(1.,0.,0.));
#14738=DIRECTION('',(0.,1.,0.));
#14739=DIRECTION('center_axis',(0.,-1.,0.));
#14740=DIRECTION('ref_axis',(1.,0.,0.));
#14741=DIRECTION('center_axis',(0.,1.,0.));
#14742=DIRECTION('ref_axis',(1.,0.,0.));
#14743=DIRECTION('center_axis',(0.,1.,0.));
#14744=DIRECTION('ref_axis',(1.,0.,0.));
#14745=DIRECTION('',(0.,1.,0.));
#14746=DIRECTION('center_axis',(0.,-1.,0.));
#14747=DIRECTION('ref_axis',(1.,0.,0.));
#14748=DIRECTION('center_axis',(0.,1.,0.));
#14749=DIRECTION('ref_axis',(1.,0.,0.));
#14750=DIRECTION('center_axis',(0.,1.,0.));
#14751=DIRECTION('ref_axis',(1.,0.,0.));
#14752=DIRECTION('',(0.,1.,0.));
#14753=DIRECTION('center_axis',(0.,-1.,0.));
#14754=DIRECTION('ref_axis',(1.,0.,0.));
#14755=DIRECTION('center_axis',(0.,1.,0.));
#14756=DIRECTION('ref_axis',(1.,0.,0.));
#14757=DIRECTION('center_axis',(0.,1.,0.));
#14758=DIRECTION('ref_axis',(1.,0.,0.));
#14759=DIRECTION('',(0.,1.,0.));
#14760=DIRECTION('center_axis',(0.,-1.,0.));
#14761=DIRECTION('ref_axis',(1.,0.,0.));
#14762=DIRECTION('center_axis',(0.,0.,1.));
#14763=DIRECTION('ref_axis',(1.,0.,0.));
#14764=DIRECTION('center_axis',(0.,0.,1.));
#14765=DIRECTION('ref_axis',(1.,0.,0.));
#14766=DIRECTION('',(0.,0.,1.));
#14767=DIRECTION('center_axis',(0.,0.,-1.));
#14768=DIRECTION('ref_axis',(1.,0.,0.));
#14769=DIRECTION('center_axis',(0.,0.,1.));
#14770=DIRECTION('ref_axis',(1.,0.,0.));
#14771=DIRECTION('center_axis',(0.,0.,1.));
#14772=DIRECTION('ref_axis',(1.,0.,0.));
#14773=DIRECTION('',(0.,0.,1.));
#14774=DIRECTION('center_axis',(0.,0.,-1.));
#14775=DIRECTION('ref_axis',(1.,0.,0.));
#14776=DIRECTION('center_axis',(0.,0.,1.));
#14777=DIRECTION('ref_axis',(1.,0.,0.));
#14778=DIRECTION('center_axis',(0.,0.,1.));
#14779=DIRECTION('ref_axis',(1.,0.,0.));
#14780=DIRECTION('',(0.,0.,1.));
#14781=DIRECTION('center_axis',(0.,0.,-1.));
#14782=DIRECTION('ref_axis',(1.,0.,0.));
#14783=DIRECTION('center_axis',(0.,0.,1.));
#14784=DIRECTION('ref_axis',(1.,0.,0.));
#14785=DIRECTION('center_axis',(0.,0.,1.));
#14786=DIRECTION('ref_axis',(1.,0.,0.));
#14787=DIRECTION('',(0.,0.,1.));
#14788=DIRECTION('center_axis',(0.,0.,-1.));
#14789=DIRECTION('ref_axis',(1.,0.,0.));
#14790=DIRECTION('center_axis',(0.,0.,1.));
#14791=DIRECTION('ref_axis',(1.,0.,0.));
#14792=DIRECTION('',(0.,1.,0.));
#14793=DIRECTION('',(-1.,0.,0.));
#14794=DIRECTION('',(0.,1.,0.));
#14795=DIRECTION('',(1.,0.,0.));
#14796=DIRECTION('center_axis',(0.,0.,1.));
#14797=DIRECTION('ref_axis',(1.,0.,0.));
#14798=DIRECTION('',(0.,-1.,0.));
#14799=DIRECTION('',(1.,0.,0.));
#14800=DIRECTION('',(0.,1.,0.));
#14801=DIRECTION('',(-1.,0.,0.));
#14802=DIRECTION('center_axis',(-1.,0.,0.));
#14803=DIRECTION('ref_axis',(0.,0.,1.));
#14804=DIRECTION('',(0.,0.,-1.));
#14805=DIRECTION('',(0.,0.,1.));
#14806=DIRECTION('',(0.,1.,0.));
#14807=DIRECTION('center_axis',(1.,0.,0.));
#14808=DIRECTION('ref_axis',(0.,0.,-1.));
#14809=DIRECTION('',(0.,0.,1.));
#14810=DIRECTION('',(0.,1.,0.));
#14811=DIRECTION('',(0.,0.,-1.));
#14812=DIRECTION('center_axis',(0.,-1.,0.));
#14813=DIRECTION('ref_axis',(1.,0.,0.));
#14814=DIRECTION('',(0.,0.,1.));
#14815=DIRECTION('',(1.,0.,0.));
#14816=DIRECTION('',(0.,0.,1.));
#14817=DIRECTION('',(1.,0.,0.));
#14818=DIRECTION('center_axis',(1.,0.,0.));
#14819=DIRECTION('ref_axis',(0.,1.,0.));
#14820=DIRECTION('',(0.,0.,1.));
#14821=DIRECTION('',(0.,1.,0.));
#14822=DIRECTION('center_axis',(0.,1.,0.));
#14823=DIRECTION('ref_axis',(-1.,0.,0.));
#14824=DIRECTION('',(0.,0.,1.));
#14825=DIRECTION('',(-1.,0.,0.));
#14826=DIRECTION('',(-1.,0.,0.));
#14827=DIRECTION('center_axis',(-1.,0.,0.));
#14828=DIRECTION('ref_axis',(0.,-1.,0.));
#14829=DIRECTION('',(0.,-1.,0.));
#14830=DIRECTION('center_axis',(0.,0.,1.));
#14831=DIRECTION('ref_axis',(1.,0.,0.));
#14832=DIRECTION('center_axis',(0.,0.,1.));
#14833=DIRECTION('ref_axis',(1.,0.,0.));
#14834=DIRECTION('axis',(0.,0.,1.));
#14835=DIRECTION('refdir',(1.,0.,0.));
#14836=DIRECTION('center_axis',(0.,1.,0.));
#14837=DIRECTION('ref_axis',(1.,0.,0.));
#14838=DIRECTION('center_axis',(0.,-1.,0.));
#14839=DIRECTION('ref_axis',(1.,0.,0.));
#14840=DIRECTION('',(0.,-1.,0.));
#14841=DIRECTION('center_axis',(0.,-1.,0.));
#14842=DIRECTION('ref_axis',(1.,0.,0.));
#14843=DIRECTION('center_axis',(0.,1.,0.));
#14844=DIRECTION('ref_axis',(1.,0.,0.));
#14845=DIRECTION('center_axis',(0.,1.,0.));
#14846=DIRECTION('ref_axis',(1.,0.,0.));
#14847=DIRECTION('',(0.,-1.,0.));
#14848=DIRECTION('center_axis',(0.,1.,0.));
#14849=DIRECTION('ref_axis',(1.,0.,0.));
#14850=DIRECTION('center_axis',(0.,1.,0.));
#14851=DIRECTION('ref_axis',(1.,0.,0.));
#14852=DIRECTION('center_axis',(0.,1.,0.));
#14853=DIRECTION('ref_axis',(1.,0.,0.));
#14854=DIRECTION('axis',(0.,0.,1.));
#14855=DIRECTION('refdir',(1.,0.,0.));
#14856=DIRECTION('center_axis',(0.,1.,0.));
#14857=DIRECTION('ref_axis',(0.707106781186546,0.,0.707106781186549));
#14858=DIRECTION('',(0.,1.,0.));
#14859=DIRECTION('center_axis',(0.,1.,0.));
#14860=DIRECTION('ref_axis',(1.,0.,0.));
#14861=DIRECTION('',(0.,-1.,0.));
#14862=DIRECTION('center_axis',(0.,-1.,0.));
#14863=DIRECTION('ref_axis',(1.,0.,0.));
#14864=DIRECTION('center_axis',(0.,1.,0.));
#14865=DIRECTION('ref_axis',(0.707106781186547,0.,-0.707106781186548));
#14866=DIRECTION('',(0.,1.,0.));
#14867=DIRECTION('center_axis',(0.,1.,0.));
#14868=DIRECTION('ref_axis',(1.,0.,0.));
#14869=DIRECTION('',(0.,-1.,0.));
#14870=DIRECTION('center_axis',(0.,-1.,0.));
#14871=DIRECTION('ref_axis',(1.,0.,0.));
#14872=DIRECTION('center_axis',(0.,1.,0.));
#14873=DIRECTION('ref_axis',(-0.707106781186552,0.,-0.707106781186543));
#14874=DIRECTION('',(0.,1.,0.));
#14875=DIRECTION('center_axis',(0.,1.,0.));
#14876=DIRECTION('ref_axis',(1.,0.,0.));
#14877=DIRECTION('',(0.,-1.,0.));
#14878=DIRECTION('center_axis',(0.,-1.,0.));
#14879=DIRECTION('ref_axis',(1.,0.,0.));
#14880=DIRECTION('center_axis',(0.,1.,0.));
#14881=DIRECTION('ref_axis',(-0.707106781186546,0.,0.707106781186549));
#14882=DIRECTION('',(0.,1.,0.));
#14883=DIRECTION('center_axis',(0.,1.,0.));
#14884=DIRECTION('ref_axis',(1.,0.,0.));
#14885=DIRECTION('',(0.,-1.,0.));
#14886=DIRECTION('center_axis',(0.,-1.,0.));
#14887=DIRECTION('ref_axis',(1.,0.,0.));
#14888=DIRECTION('center_axis',(0.,1.,0.));
#14889=DIRECTION('ref_axis',(1.,0.,0.));
#14890=DIRECTION('center_axis',(0.,1.,0.));
#14891=DIRECTION('ref_axis',(1.,0.,0.));
#14892=DIRECTION('center_axis',(0.,1.,0.));
#14893=DIRECTION('ref_axis',(1.,0.,0.));
#14894=DIRECTION('center_axis',(0.,1.,0.));
#14895=DIRECTION('ref_axis',(1.,0.,0.));
#14896=DIRECTION('center_axis',(0.,1.,0.));
#14897=DIRECTION('ref_axis',(1.,0.,0.));
#14898=DIRECTION('center_axis',(0.,-1.,0.));
#14899=DIRECTION('ref_axis',(1.,0.,0.));
#14900=DIRECTION('center_axis',(0.,1.,0.));
#14901=DIRECTION('ref_axis',(1.,0.,0.));
#14902=DIRECTION('center_axis',(0.,1.,0.));
#14903=DIRECTION('ref_axis',(1.,0.,0.));
#14904=DIRECTION('center_axis',(0.,1.,0.));
#14905=DIRECTION('ref_axis',(1.,0.,0.));
#14906=DIRECTION('center_axis',(0.,1.,0.));
#14907=DIRECTION('ref_axis',(1.,0.,0.));
#14908=DIRECTION('center_axis',(0.,1.,0.));
#14909=DIRECTION('ref_axis',(1.,0.,0.));
#14910=DIRECTION('center_axis',(0.,1.,0.));
#14911=DIRECTION('ref_axis',(1.,0.,0.));
#14912=DIRECTION('center_axis',(0.,1.,0.));
#14913=DIRECTION('ref_axis',(-1.,0.,-1.22464679914735E-16));
#14914=DIRECTION('center_axis',(0.,1.,0.));
#14915=DIRECTION('ref_axis',(1.,0.,0.));
#14916=DIRECTION('center_axis',(0.,1.,0.));
#14917=DIRECTION('ref_axis',(1.,0.,0.));
#14918=DIRECTION('center_axis',(0.,1.,0.));
#14919=DIRECTION('ref_axis',(1.,0.,0.));
#14920=DIRECTION('',(0.,-1.,0.));
#14921=DIRECTION('center_axis',(0.,-1.,0.));
#14922=DIRECTION('ref_axis',(1.,0.,0.));
#14923=DIRECTION('center_axis',(0.,1.,0.));
#14924=DIRECTION('ref_axis',(1.,0.,0.));
#14925=DIRECTION('center_axis',(0.,-1.,0.));
#14926=DIRECTION('ref_axis',(1.,0.,0.));
#14927=DIRECTION('center_axis',(0.,1.,0.));
#14928=DIRECTION('ref_axis',(1.,0.,0.));
#14929=DIRECTION('',(0.,-1.,0.));
#14930=DIRECTION('center_axis',(0.,1.,0.));
#14931=DIRECTION('ref_axis',(1.,0.,0.));
#14932=DIRECTION('axis',(0.,0.,1.));
#14933=DIRECTION('refdir',(1.,0.,0.));
#14934=DIRECTION('center_axis',(0.,1.,0.));
#14935=DIRECTION('ref_axis',(0.707106781186546,0.,0.707106781186549));
#14936=DIRECTION('',(0.,1.,0.));
#14937=DIRECTION('center_axis',(0.,1.,0.));
#14938=DIRECTION('ref_axis',(1.,0.,0.));
#14939=DIRECTION('',(0.,-1.,0.));
#14940=DIRECTION('center_axis',(0.,-1.,0.));
#14941=DIRECTION('ref_axis',(1.,0.,0.));
#14942=DIRECTION('center_axis',(0.,1.,0.));
#14943=DIRECTION('ref_axis',(0.707106781186547,0.,-0.707106781186548));
#14944=DIRECTION('',(0.,1.,0.));
#14945=DIRECTION('center_axis',(0.,1.,0.));
#14946=DIRECTION('ref_axis',(1.,0.,0.));
#14947=DIRECTION('',(0.,-1.,0.));
#14948=DIRECTION('center_axis',(0.,-1.,0.));
#14949=DIRECTION('ref_axis',(1.,0.,0.));
#14950=DIRECTION('center_axis',(0.,1.,0.));
#14951=DIRECTION('ref_axis',(-0.707106781186552,0.,-0.707106781186543));
#14952=DIRECTION('',(0.,1.,0.));
#14953=DIRECTION('center_axis',(0.,1.,0.));
#14954=DIRECTION('ref_axis',(1.,0.,0.));
#14955=DIRECTION('',(0.,-1.,0.));
#14956=DIRECTION('center_axis',(0.,-1.,0.));
#14957=DIRECTION('ref_axis',(1.,0.,0.));
#14958=DIRECTION('center_axis',(0.,1.,0.));
#14959=DIRECTION('ref_axis',(-0.707106781186546,0.,0.707106781186549));
#14960=DIRECTION('',(0.,1.,0.));
#14961=DIRECTION('center_axis',(0.,1.,0.));
#14962=DIRECTION('ref_axis',(1.,0.,0.));
#14963=DIRECTION('',(0.,-1.,0.));
#14964=DIRECTION('center_axis',(0.,-1.,0.));
#14965=DIRECTION('ref_axis',(1.,0.,0.));
#14966=DIRECTION('center_axis',(0.,1.,0.));
#14967=DIRECTION('ref_axis',(1.,0.,0.));
#14968=DIRECTION('center_axis',(0.,1.,0.));
#14969=DIRECTION('ref_axis',(1.,0.,0.));
#14970=DIRECTION('center_axis',(0.,1.,0.));
#14971=DIRECTION('ref_axis',(1.,0.,0.));
#14972=DIRECTION('center_axis',(0.,1.,0.));
#14973=DIRECTION('ref_axis',(1.,0.,0.));
#14974=DIRECTION('center_axis',(0.,1.,0.));
#14975=DIRECTION('ref_axis',(1.,0.,0.));
#14976=DIRECTION('center_axis',(0.,1.,0.));
#14977=DIRECTION('ref_axis',(1.,0.,0.));
#14978=DIRECTION('center_axis',(0.,1.,0.));
#14979=DIRECTION('ref_axis',(1.,0.,0.));
#14980=DIRECTION('center_axis',(0.,1.,0.));
#14981=DIRECTION('ref_axis',(1.,0.,0.));
#14982=DIRECTION('center_axis',(0.,1.,0.));
#14983=DIRECTION('ref_axis',(1.,0.,0.));
#14984=DIRECTION('center_axis',(0.,1.,0.));
#14985=DIRECTION('ref_axis',(1.,0.,0.));
#14986=DIRECTION('center_axis',(0.,1.,0.));
#14987=DIRECTION('ref_axis',(1.,0.,0.));
#14988=DIRECTION('center_axis',(0.,1.,0.));
#14989=DIRECTION('ref_axis',(1.,0.,0.));
#14990=DIRECTION('center_axis',(0.,1.,0.));
#14991=DIRECTION('ref_axis',(-1.,0.,-1.22464679914735E-16));
#14992=DIRECTION('center_axis',(0.,1.,0.));
#14993=DIRECTION('ref_axis',(1.,0.,0.));
#14994=DIRECTION('center_axis',(0.,1.,0.));
#14995=DIRECTION('ref_axis',(1.,0.,0.));
#14996=DIRECTION('',(0.,-1.,0.));
#14997=DIRECTION('center_axis',(0.,1.,0.));
#14998=DIRECTION('ref_axis',(1.,0.,0.));
#14999=DIRECTION('center_axis',(0.,1.,0.));
#15000=DIRECTION('ref_axis',(1.,0.,0.));
#15001=DIRECTION('center_axis',(0.,-1.,0.));
#15002=DIRECTION('ref_axis',(1.,0.,0.));
#15003=DIRECTION('center_axis',(0.,1.,0.));
#15004=DIRECTION('ref_axis',(1.,0.,0.));
#15005=DIRECTION('center_axis',(0.,-1.,0.));
#15006=DIRECTION('ref_axis',(1.,0.,0.));
#15007=DIRECTION('',(0.,-1.,0.));
#15008=DIRECTION('center_axis',(0.,1.,0.));
#15009=DIRECTION('ref_axis',(1.,0.,0.));
#15010=DIRECTION('axis',(0.,0.,1.));
#15011=DIRECTION('refdir',(1.,0.,0.));
#15012=DIRECTION('center_axis',(0.,0.,1.));
#15013=DIRECTION('ref_axis',(1.,0.,0.));
#15014=DIRECTION('center_axis',(0.,0.,1.));
#15015=DIRECTION('ref_axis',(1.,0.,0.));
#15016=DIRECTION('',(0.,0.,1.));
#15017=DIRECTION('center_axis',(0.,0.,-1.));
#15018=DIRECTION('ref_axis',(1.,0.,0.));
#15019=DIRECTION('center_axis',(0.,0.,1.));
#15020=DIRECTION('ref_axis',(1.,0.,0.));
#15021=DIRECTION('center_axis',(0.,0.,1.));
#15022=DIRECTION('ref_axis',(1.,0.,0.));
#15023=DIRECTION('center_axis',(0.,0.,1.));
#15024=DIRECTION('ref_axis',(1.,0.,0.));
#15025=DIRECTION('center_axis',(0.,0.,1.));
#15026=DIRECTION('ref_axis',(1.,0.,0.));
#15027=DIRECTION('',(0.,0.,1.));
#15028=DIRECTION('center_axis',(0.,0.,-1.));
#15029=DIRECTION('ref_axis',(1.,0.,0.));
#15030=DIRECTION('center_axis',(0.,0.,1.));
#15031=DIRECTION('ref_axis',(1.,0.,0.));
#15032=DIRECTION('center_axis',(0.,0.,1.));
#15033=DIRECTION('ref_axis',(1.,0.,0.));
#15034=DIRECTION('center_axis',(0.,0.,1.));
#15035=DIRECTION('ref_axis',(1.,0.,0.));
#15036=DIRECTION('center_axis',(0.,0.,1.));
#15037=DIRECTION('ref_axis',(1.,0.,0.));
#15038=DIRECTION('',(0.,0.,1.));
#15039=DIRECTION('center_axis',(0.,0.,1.));
#15040=DIRECTION('ref_axis',(1.,0.,0.));
#15041=DIRECTION('center_axis',(0.,0.,1.));
#15042=DIRECTION('ref_axis',(1.,0.,0.));
#15043=DIRECTION('',(0.,0.,1.));
#15044=DIRECTION('center_axis',(1.,0.,0.));
#15045=DIRECTION('ref_axis',(0.,0.,-1.));
#15046=DIRECTION('center_axis',(1.,0.,0.));
#15047=DIRECTION('ref_axis',(0.,0.,-1.));
#15048=DIRECTION('',(1.,0.,0.));
#15049=DIRECTION('center_axis',(-1.,0.,0.));
#15050=DIRECTION('ref_axis',(0.,0.,-1.));
#15051=DIRECTION('center_axis',(0.,1.,0.));
#15052=DIRECTION('ref_axis',(-1.,0.,0.));
#15053=DIRECTION('',(-1.,0.,0.));
#15054=DIRECTION('',(0.,0.,1.));
#15055=DIRECTION('',(-1.,0.,0.));
#15056=DIRECTION('',(0.,0.,1.));
#15057=DIRECTION('center_axis',(1.,0.,0.));
#15058=DIRECTION('ref_axis',(0.,1.,0.));
#15059=DIRECTION('',(0.,1.,0.));
#15060=DIRECTION('',(0.,1.,0.));
#15061=DIRECTION('',(0.,0.,1.));
#15062=DIRECTION('center_axis',(0.,-1.,0.));
#15063=DIRECTION('ref_axis',(1.,0.,0.));
#15064=DIRECTION('',(1.,0.,0.));
#15065=DIRECTION('',(1.,0.,0.));
#15066=DIRECTION('',(0.,0.,1.));
#15067=DIRECTION('center_axis',(-1.,0.,0.));
#15068=DIRECTION('ref_axis',(0.,-1.,0.));
#15069=DIRECTION('',(0.,-1.,0.));
#15070=DIRECTION('',(0.,-1.,0.));
#15071=DIRECTION('center_axis',(0.,0.,1.));
#15072=DIRECTION('ref_axis',(1.,0.,0.));
#15073=DIRECTION('center_axis',(0.,0.,1.));
#15074=DIRECTION('ref_axis',(1.,0.,0.));
#15075=DIRECTION('axis',(0.,0.,1.));
#15076=DIRECTION('refdir',(1.,0.,0.));
#15077=DIRECTION('center_axis',(1.,0.,0.));
#15078=DIRECTION('ref_axis',(0.,0.,-1.));
#15079=DIRECTION('center_axis',(-1.,0.,0.));
#15080=DIRECTION('ref_axis',(0.,0.,-1.));
#15081=DIRECTION('',(-1.,0.,0.));
#15082=DIRECTION('center_axis',(-1.,0.,0.));
#15083=DIRECTION('ref_axis',(0.,0.,-1.));
#15084=DIRECTION('center_axis',(1.,0.,0.));
#15085=DIRECTION('ref_axis',(0.,0.,-1.));
#15086=DIRECTION('center_axis',(1.,0.,0.));
#15087=DIRECTION('ref_axis',(0.,0.,-1.));
#15088=DIRECTION('',(-1.,0.,0.));
#15089=DIRECTION('center_axis',(1.,0.,0.));
#15090=DIRECTION('ref_axis',(0.,0.,-1.));
#15091=DIRECTION('center_axis',(1.,0.,0.));
#15092=DIRECTION('ref_axis',(0.,0.,-1.));
#15093=DIRECTION('center_axis',(1.,0.,0.));
#15094=DIRECTION('ref_axis',(0.,0.,-1.));
#15095=DIRECTION('axis',(0.,0.,1.));
#15096=DIRECTION('refdir',(1.,0.,0.));
#15097=DIRECTION('center_axis',(0.,0.,1.));
#15098=DIRECTION('ref_axis',(1.,0.,0.));
#15099=DIRECTION('center_axis',(0.,0.,1.));
#15100=DIRECTION('ref_axis',(1.,0.,0.));
#15101=DIRECTION('',(0.,0.,1.));
#15102=DIRECTION('center_axis',(0.,0.,-1.));
#15103=DIRECTION('ref_axis',(1.,0.,0.));
#15104=DIRECTION('center_axis',(0.,0.,1.));
#15105=DIRECTION('ref_axis',(1.,0.,0.));
#15106=DIRECTION('center_axis',(0.,0.,1.));
#15107=DIRECTION('ref_axis',(1.,0.,0.));
#15108=DIRECTION('center_axis',(0.,0.,1.));
#15109=DIRECTION('ref_axis',(1.,0.,0.));
#15110=DIRECTION('center_axis',(0.,0.,1.));
#15111=DIRECTION('ref_axis',(1.,0.,0.));
#15112=DIRECTION('',(0.,0.,1.));
#15113=DIRECTION('center_axis',(0.,0.,-1.));
#15114=DIRECTION('ref_axis',(1.,0.,0.));
#15115=DIRECTION('center_axis',(0.,0.,1.));
#15116=DIRECTION('ref_axis',(1.,0.,0.));
#15117=DIRECTION('center_axis',(0.,0.,1.));
#15118=DIRECTION('ref_axis',(1.,0.,0.));
#15119=DIRECTION('center_axis',(0.,0.,1.));
#15120=DIRECTION('ref_axis',(1.,0.,0.));
#15121=DIRECTION('center_axis',(0.,0.,1.));
#15122=DIRECTION('ref_axis',(1.,0.,0.));
#15123=DIRECTION('',(0.,0.,1.));
#15124=DIRECTION('center_axis',(0.,0.,1.));
#15125=DIRECTION('ref_axis',(1.,0.,0.));
#15126=DIRECTION('center_axis',(0.,0.,1.));
#15127=DIRECTION('ref_axis',(1.,0.,0.));
#15128=DIRECTION('',(0.,0.,1.));
#15129=DIRECTION('center_axis',(1.,0.,0.));
#15130=DIRECTION('ref_axis',(0.,0.,-1.));
#15131=DIRECTION('center_axis',(1.,0.,0.));
#15132=DIRECTION('ref_axis',(0.,0.,-1.));
#15133=DIRECTION('',(1.,0.,0.));
#15134=DIRECTION('center_axis',(-1.,0.,0.));
#15135=DIRECTION('ref_axis',(0.,0.,-1.));
#15136=DIRECTION('center_axis',(0.,1.,0.));
#15137=DIRECTION('ref_axis',(-1.,0.,0.));
#15138=DIRECTION('',(-1.,0.,0.));
#15139=DIRECTION('',(0.,0.,1.));
#15140=DIRECTION('',(-1.,0.,0.));
#15141=DIRECTION('',(0.,0.,1.));
#15142=DIRECTION('center_axis',(1.,0.,0.));
#15143=DIRECTION('ref_axis',(0.,1.,0.));
#15144=DIRECTION('',(0.,1.,0.));
#15145=DIRECTION('',(0.,1.,0.));
#15146=DIRECTION('',(0.,0.,1.));
#15147=DIRECTION('center_axis',(0.,-1.,0.));
#15148=DIRECTION('ref_axis',(1.,0.,0.));
#15149=DIRECTION('',(1.,0.,0.));
#15150=DIRECTION('',(1.,0.,0.));
#15151=DIRECTION('',(0.,0.,1.));
#15152=DIRECTION('center_axis',(-1.,0.,0.));
#15153=DIRECTION('ref_axis',(0.,-1.,0.));
#15154=DIRECTION('',(0.,-1.,0.));
#15155=DIRECTION('',(0.,-1.,0.));
#15156=DIRECTION('center_axis',(0.,0.,1.));
#15157=DIRECTION('ref_axis',(1.,0.,0.));
#15158=DIRECTION('center_axis',(0.,0.,1.));
#15159=DIRECTION('ref_axis',(1.,0.,0.));
#15160=DIRECTION('axis',(0.,0.,1.));
#15161=DIRECTION('refdir',(1.,0.,0.));
#15162=DIRECTION('center_axis',(1.,0.,0.));
#15163=DIRECTION('ref_axis',(0.,0.,-1.));
#15164=DIRECTION('center_axis',(-1.,0.,0.));
#15165=DIRECTION('ref_axis',(0.,0.,-1.));
#15166=DIRECTION('',(-1.,0.,0.));
#15167=DIRECTION('center_axis',(-1.,0.,0.));
#15168=DIRECTION('ref_axis',(0.,0.,-1.));
#15169=DIRECTION('center_axis',(1.,0.,0.));
#15170=DIRECTION('ref_axis',(0.,0.,-1.));
#15171=DIRECTION('center_axis',(1.,0.,0.));
#15172=DIRECTION('ref_axis',(0.,0.,-1.));
#15173=DIRECTION('',(-1.,0.,0.));
#15174=DIRECTION('center_axis',(1.,0.,0.));
#15175=DIRECTION('ref_axis',(0.,0.,-1.));
#15176=DIRECTION('center_axis',(1.,0.,0.));
#15177=DIRECTION('ref_axis',(0.,0.,-1.));
#15178=DIRECTION('center_axis',(1.,0.,0.));
#15179=DIRECTION('ref_axis',(0.,0.,-1.));
#15180=DIRECTION('axis',(0.,0.,1.));
#15181=DIRECTION('refdir',(1.,0.,0.));
#15182=DIRECTION('center_axis',(1.,0.,0.));
#15183=DIRECTION('ref_axis',(0.,0.,-1.));
#15184=DIRECTION('center_axis',(-1.,0.,0.));
#15185=DIRECTION('ref_axis',(0.,0.,-1.));
#15186=DIRECTION('',(-1.,0.,0.));
#15187=DIRECTION('center_axis',(-1.,0.,0.));
#15188=DIRECTION('ref_axis',(0.,0.,-1.));
#15189=DIRECTION('center_axis',(1.,0.,0.));
#15190=DIRECTION('ref_axis',(0.,0.,-1.));
#15191=DIRECTION('center_axis',(1.,0.,0.));
#15192=DIRECTION('ref_axis',(0.,0.,-1.));
#15193=DIRECTION('',(-1.,0.,0.));
#15194=DIRECTION('center_axis',(1.,0.,0.));
#15195=DIRECTION('ref_axis',(0.,0.,-1.));
#15196=DIRECTION('center_axis',(1.,0.,0.));
#15197=DIRECTION('ref_axis',(0.,0.,-1.));
#15198=DIRECTION('center_axis',(1.,0.,0.));
#15199=DIRECTION('ref_axis',(0.,0.,-1.));
#15200=DIRECTION('axis',(0.,0.,1.));
#15201=DIRECTION('refdir',(1.,0.,0.));
#15202=DIRECTION('center_axis',(0.,0.,1.));
#15203=DIRECTION('ref_axis',(1.,0.,0.));
#15204=DIRECTION('',(0.,0.,1.));
#15205=DIRECTION('center_axis',(0.,0.,1.));
#15206=DIRECTION('ref_axis',(1.,0.,0.));
#15207=DIRECTION('',(0.,0.,1.));
#15208=DIRECTION('center_axis',(0.,0.,-1.));
#15209=DIRECTION('ref_axis',(1.,0.,0.));
#15210=DIRECTION('center_axis',(0.,0.,1.));
#15211=DIRECTION('ref_axis',(1.,0.,0.));
#15212=DIRECTION('',(0.,0.,1.));
#15213=DIRECTION('center_axis',(0.,0.,1.));
#15214=DIRECTION('ref_axis',(1.,0.,0.));
#15215=DIRECTION('',(0.,0.,1.));
#15216=DIRECTION('center_axis',(0.,0.,-1.));
#15217=DIRECTION('ref_axis',(1.,0.,0.));
#15218=DIRECTION('center_axis',(0.,0.,1.));
#15219=DIRECTION('ref_axis',(1.,0.,0.));
#15220=DIRECTION('center_axis',(0.,0.,-1.));
#15221=DIRECTION('ref_axis',(1.,0.,0.));
#15222=DIRECTION('',(0.,0.,1.));
#15223=DIRECTION('center_axis',(0.,0.,1.));
#15224=DIRECTION('ref_axis',(1.,0.,0.));
#15225=DIRECTION('center_axis',(0.,0.,1.));
#15226=DIRECTION('ref_axis',(1.,0.,0.));
#15227=DIRECTION('center_axis',(0.,0.,1.));
#15228=DIRECTION('ref_axis',(1.,0.,0.));
#15229=DIRECTION('center_axis',(0.,0.,1.));
#15230=DIRECTION('ref_axis',(1.,0.,0.));
#15231=DIRECTION('center_axis',(0.,0.,-1.));
#15232=DIRECTION('ref_axis',(1.,0.,0.));
#15233=DIRECTION('',(0.,0.,1.));
#15234=DIRECTION('center_axis',(0.,0.,1.));
#15235=DIRECTION('ref_axis',(1.,0.,0.));
#15236=DIRECTION('center_axis',(0.,0.,1.));
#15237=DIRECTION('ref_axis',(1.,0.,0.));
#15238=DIRECTION('center_axis',(0.,0.,1.));
#15239=DIRECTION('ref_axis',(1.,0.,0.));
#15240=DIRECTION('center_axis',(0.,0.,1.));
#15241=DIRECTION('ref_axis',(1.,0.,0.));
#15242=DIRECTION('',(-1.,0.,0.));
#15243=DIRECTION('',(0.,-1.,0.));
#15244=DIRECTION('',(1.,0.,0.));
#15245=DIRECTION('center_axis',(0.,0.,1.));
#15246=DIRECTION('ref_axis',(1.,0.,0.));
#15247=DIRECTION('',(1.,0.,0.));
#15248=DIRECTION('',(0.,1.,0.));
#15249=DIRECTION('',(-1.,0.,0.));
#15250=DIRECTION('center_axis',(0.,0.,1.));
#15251=DIRECTION('ref_axis',(1.,0.,0.));
#15252=DIRECTION('',(-1.,0.,0.));
#15253=DIRECTION('',(0.,-1.,0.));
#15254=DIRECTION('',(1.,0.,0.));
#15255=DIRECTION('center_axis',(0.,0.,1.));
#15256=DIRECTION('ref_axis',(1.,0.,0.));
#15257=DIRECTION('center_axis',(0.,0.,1.));
#15258=DIRECTION('ref_axis',(1.,0.,0.));
#15259=DIRECTION('',(0.,0.,1.));
#15260=DIRECTION('center_axis',(0.,0.,1.));
#15261=DIRECTION('ref_axis',(1.,0.,0.));
#15262=DIRECTION('center_axis',(0.,0.,1.));
#15263=DIRECTION('ref_axis',(1.,0.,0.));
#15264=DIRECTION('',(0.,0.,1.));
#15265=DIRECTION('center_axis',(1.,0.,0.));
#15266=DIRECTION('ref_axis',(0.,0.,-1.));
#15267=DIRECTION('',(-1.,0.,0.));
#15268=DIRECTION('center_axis',(-1.,0.,0.));
#15269=DIRECTION('ref_axis',(0.,0.,-1.));
#15270=DIRECTION('center_axis',(1.,0.,0.));
#15271=DIRECTION('ref_axis',(0.,0.,-1.));
#15272=DIRECTION('center_axis',(1.,0.,0.));
#15273=DIRECTION('ref_axis',(0.,1.,0.));
#15274=DIRECTION('',(0.,1.,0.));
#15275=DIRECTION('',(0.,0.,1.));
#15276=DIRECTION('',(0.,1.,0.));
#15277=DIRECTION('',(0.,0.,1.));
#15278=DIRECTION('center_axis',(0.,0.,1.));
#15279=DIRECTION('ref_axis',(1.,0.,0.));
#15280=DIRECTION('',(1.,0.,0.));
#15281=DIRECTION('center_axis',(0.,1.,0.));
#15282=DIRECTION('ref_axis',(-1.,0.,0.));
#15283=DIRECTION('',(-1.,0.,0.));
#15284=DIRECTION('',(0.,0.,1.));
#15285=DIRECTION('center_axis',(0.,-1.,0.));
#15286=DIRECTION('ref_axis',(1.,0.,0.));
#15287=DIRECTION('',(1.,0.,0.));
#15288=DIRECTION('',(0.,0.,1.));
#15289=DIRECTION('center_axis',(-1.,0.,0.));
#15290=DIRECTION('ref_axis',(0.,-1.,0.));
#15291=DIRECTION('',(0.,-1.,0.));
#15292=DIRECTION('center_axis',(0.,0.,1.));
#15293=DIRECTION('ref_axis',(1.,0.,0.));
#15294=DIRECTION('axis',(0.,0.,1.));
#15295=DIRECTION('refdir',(1.,0.,0.));
#15296=DIRECTION('center_axis',(0.,0.,1.));
#15297=DIRECTION('ref_axis',(1.,0.,0.));
#15298=DIRECTION('center_axis',(0.,0.,1.));
#15299=DIRECTION('ref_axis',(1.,0.,0.));
#15300=DIRECTION('',(0.,0.,1.));
#15301=DIRECTION('center_axis',(0.,0.,-1.));
#15302=DIRECTION('ref_axis',(1.,0.,0.));
#15303=DIRECTION('center_axis',(0.,0.,1.));
#15304=DIRECTION('ref_axis',(1.,0.,0.));
#15305=DIRECTION('center_axis',(0.,0.,1.));
#15306=DIRECTION('ref_axis',(1.,0.,0.));
#15307=DIRECTION('center_axis',(0.,0.,1.));
#15308=DIRECTION('ref_axis',(1.,0.,0.));
#15309=DIRECTION('center_axis',(0.,0.,1.));
#15310=DIRECTION('ref_axis',(1.,0.,0.));
#15311=DIRECTION('',(0.,0.,1.));
#15312=DIRECTION('center_axis',(0.,0.,-1.));
#15313=DIRECTION('ref_axis',(1.,0.,0.));
#15314=DIRECTION('center_axis',(0.,0.,1.));
#15315=DIRECTION('ref_axis',(1.,0.,0.));
#15316=DIRECTION('center_axis',(0.,0.,1.));
#15317=DIRECTION('ref_axis',(1.,0.,0.));
#15318=DIRECTION('center_axis',(0.,0.,1.));
#15319=DIRECTION('ref_axis',(1.,0.,0.));
#15320=DIRECTION('center_axis',(0.,0.,1.));
#15321=DIRECTION('ref_axis',(1.,0.,0.));
#15322=DIRECTION('',(0.,0.,1.));
#15323=DIRECTION('center_axis',(0.,0.,-1.));
#15324=DIRECTION('ref_axis',(1.,0.,0.));
#15325=DIRECTION('center_axis',(0.,0.,1.));
#15326=DIRECTION('ref_axis',(1.,0.,0.));
#15327=DIRECTION('center_axis',(0.,0.,1.));
#15328=DIRECTION('ref_axis',(1.,0.,0.));
#15329=DIRECTION('center_axis',(0.,0.,1.));
#15330=DIRECTION('ref_axis',(1.,0.,0.));
#15331=DIRECTION('center_axis',(0.,0.,1.));
#15332=DIRECTION('ref_axis',(1.,0.,0.));
#15333=DIRECTION('',(0.,0.,1.));
#15334=DIRECTION('center_axis',(0.,0.,-1.));
#15335=DIRECTION('ref_axis',(1.,0.,0.));
#15336=DIRECTION('center_axis',(0.,0.,1.));
#15337=DIRECTION('ref_axis',(1.,0.,0.));
#15338=DIRECTION('center_axis',(0.,0.,1.));
#15339=DIRECTION('ref_axis',(1.,0.,0.));
#15340=DIRECTION('center_axis',(0.,0.,1.));
#15341=DIRECTION('ref_axis',(1.,0.,0.));
#15342=DIRECTION('center_axis',(0.,0.,1.));
#15343=DIRECTION('ref_axis',(1.,0.,0.));
#15344=DIRECTION('',(0.,0.,1.));
#15345=DIRECTION('center_axis',(0.,0.,1.));
#15346=DIRECTION('ref_axis',(1.,0.,0.));
#15347=DIRECTION('center_axis',(0.,0.,1.));
#15348=DIRECTION('ref_axis',(1.,0.,0.));
#15349=DIRECTION('',(0.,0.,1.));
#15350=DIRECTION('center_axis',(0.,0.,1.));
#15351=DIRECTION('ref_axis',(1.,0.,0.));
#15352=DIRECTION('center_axis',(0.,0.,1.));
#15353=DIRECTION('ref_axis',(1.,0.,0.));
#15354=DIRECTION('',(0.,0.,1.));
#15355=DIRECTION('center_axis',(0.,0.,1.));
#15356=DIRECTION('ref_axis',(1.,0.,0.));
#15357=DIRECTION('center_axis',(0.,0.,1.));
#15358=DIRECTION('ref_axis',(1.,0.,0.));
#15359=DIRECTION('',(0.,0.,1.));
#15360=DIRECTION('center_axis',(0.,-0.56333682464151,0.826227342807548));
#15361=DIRECTION('ref_axis',(0.,-0.826227342807548,-0.56333682464151));
#15362=DIRECTION('',(0.,-0.826227342807548,-0.56333682464151));
#15363=DIRECTION('',(1.,0.,0.));
#15364=DIRECTION('',(0.,-0.826227342807548,-0.56333682464151));
#15365=DIRECTION('',(1.,0.,0.));
#15366=DIRECTION('center_axis',(0.,-1.,0.));
#15367=DIRECTION('ref_axis',(0.,0.,-1.));
#15368=DIRECTION('',(0.,0.,-1.));
#15369=DIRECTION('',(0.,0.,-1.));
#15370=DIRECTION('',(1.,0.,0.));
#15371=DIRECTION('center_axis',(0.,-0.56333682464151,-0.826227342807548));
#15372=DIRECTION('ref_axis',(0.,0.826227342807548,-0.56333682464151));
#15373=DIRECTION('',(0.,0.826227342807548,-0.56333682464151));
#15374=DIRECTION('',(0.,0.826227342807548,-0.56333682464151));
#15375=DIRECTION('',(1.,0.,0.));
#15376=DIRECTION('center_axis',(0.,-1.,0.));
#15377=DIRECTION('ref_axis',(0.,0.,-1.));
#15378=DIRECTION('',(0.,0.,-1.));
#15379=DIRECTION('',(0.,0.,-1.));
#15380=DIRECTION('',(1.,0.,0.));
#15381=DIRECTION('center_axis',(0.,0.,1.));
#15382=DIRECTION('ref_axis',(0.,-1.,0.));
#15383=DIRECTION('',(0.,-1.,0.));
#15384=DIRECTION('',(0.,-1.,0.));
#15385=DIRECTION('',(1.,0.,0.));
#15386=DIRECTION('center_axis',(0.,1.,0.));
#15387=DIRECTION('ref_axis',(0.,0.,1.));
#15388=DIRECTION('',(0.,0.,1.));
#15389=DIRECTION('',(0.,0.,1.));
#15390=DIRECTION('',(1.,0.,0.));
#15391=DIRECTION('center_axis',(0.,0.56333682464151,-0.826227342807548));
#15392=DIRECTION('ref_axis',(0.,0.826227342807548,0.56333682464151));
#15393=DIRECTION('',(0.,0.826227342807548,0.56333682464151));
#15394=DIRECTION('',(0.,0.826227342807548,0.56333682464151));
#15395=DIRECTION('',(1.,0.,0.));
#15396=DIRECTION('center_axis',(0.,1.,0.));
#15397=DIRECTION('ref_axis',(0.,0.,1.));
#15398=DIRECTION('',(0.,0.,1.));
#15399=DIRECTION('',(0.,0.,1.));
#15400=DIRECTION('',(1.,0.,0.));
#15401=DIRECTION('center_axis',(0.,0.56333682464151,0.826227342807548));
#15402=DIRECTION('ref_axis',(0.,-0.826227342807548,0.56333682464151));
#15403=DIRECTION('',(0.,-0.826227342807548,0.56333682464151));
#15404=DIRECTION('',(0.,-0.826227342807548,0.56333682464151));
#15405=DIRECTION('',(1.,0.,0.));
#15406=DIRECTION('center_axis',(0.,1.,0.));
#15407=DIRECTION('ref_axis',(0.,0.,1.));
#15408=DIRECTION('',(0.,0.,1.));
#15409=DIRECTION('',(0.,0.,1.));
#15410=DIRECTION('',(1.,0.,0.));
#15411=DIRECTION('center_axis',(0.,0.,-1.));
#15412=DIRECTION('ref_axis',(0.,1.,0.));
#15413=DIRECTION('',(0.,1.,0.));
#15414=DIRECTION('',(0.,1.,0.));
#15415=DIRECTION('',(1.,0.,0.));
#15416=DIRECTION('center_axis',(0.,-1.,0.));
#15417=DIRECTION('ref_axis',(0.,0.,-1.));
#15418=DIRECTION('',(0.,0.,-1.));
#15419=DIRECTION('',(0.,0.,-1.));
#15420=DIRECTION('center_axis',(1.,0.,0.));
#15421=DIRECTION('ref_axis',(0.,0.,-1.));
#15422=DIRECTION('center_axis',(1.,0.,0.));
#15423=DIRECTION('ref_axis',(0.,0.,-1.));
#15424=DIRECTION('axis',(0.,0.,1.));
#15425=DIRECTION('refdir',(1.,0.,0.));
#15426=DIRECTION('axis',(0.,0.,1.));
#15427=DIRECTION('refdir',(1.,0.,0.));
#15428=DIRECTION('center_axis',(0.,-1.,0.));
#15429=DIRECTION('ref_axis',(0.,0.,-1.));
#15430=DIRECTION('center_axis',(0.,-1.,0.));
#15431=DIRECTION('ref_axis',(1.,0.,0.));
#15432=DIRECTION('center_axis',(0.,-1.,0.));
#15433=DIRECTION('ref_axis',(1.,0.,0.));
#15434=DIRECTION('center_axis',(1.,0.,1.22464679914735E-16));
#15435=DIRECTION('ref_axis',(-1.22464679914735E-16,0.,1.));
#15436=DIRECTION('center_axis',(0.,1.,0.));
#15437=DIRECTION('ref_axis',(1.,0.,0.));
#15438=DIRECTION('center_axis',(0.,1.,0.));
#15439=DIRECTION('ref_axis',(1.,0.,0.));
#15440=DIRECTION('center_axis',(0.,-1.,0.));
#15441=DIRECTION('ref_axis',(1.,0.,0.));
#15442=DIRECTION('',(0.,1.,0.));
#15443=DIRECTION('center_axis',(0.,-1.,0.));
#15444=DIRECTION('ref_axis',(1.,0.,0.));
#15445=DIRECTION('center_axis',(0.,-1.,0.));
#15446=DIRECTION('ref_axis',(1.,0.,0.));
#15447=DIRECTION('center_axis',(0.,-1.,0.));
#15448=DIRECTION('ref_axis',(1.,0.,0.));
#15449=DIRECTION('',(0.,1.,0.));
#15450=DIRECTION('center_axis',(0.,-1.,0.));
#15451=DIRECTION('ref_axis',(1.,0.,0.));
#15452=DIRECTION('center_axis',(0.,1.,0.));
#15453=DIRECTION('ref_axis',(1.,0.,0.));
#15454=DIRECTION('',(-0.707106781186547,0.707106781186548,-8.65956056235493E-17));
#15455=DIRECTION('center_axis',(0.,-1.,0.));
#15456=DIRECTION('ref_axis',(1.,0.,0.));
#15457=DIRECTION('center_axis',(0.,1.,0.));
#15458=DIRECTION('ref_axis',(0.,0.,1.));
#15459=DIRECTION('center_axis',(0.,-1.,0.));
#15460=DIRECTION('ref_axis',(1.,0.,0.));
#15461=DIRECTION('center_axis',(0.,-1.,0.));
#15462=DIRECTION('ref_axis',(1.,0.,0.));
#15463=DIRECTION('',(0.,1.,0.));
#15464=DIRECTION('center_axis',(0.,-1.,0.));
#15465=DIRECTION('ref_axis',(0.,0.,-1.));
#15466=DIRECTION('center_axis',(0.,-1.,0.));
#15467=DIRECTION('ref_axis',(1.,0.,0.));
#15468=DIRECTION('center_axis',(0.,-1.,0.));
#15469=DIRECTION('ref_axis',(1.,0.,0.));
#15470=DIRECTION('',(0.707106781186547,0.707106781186548,8.65956056235493E-17));
#15471=DIRECTION('axis',(0.,0.,1.));
#15472=DIRECTION('refdir',(1.,0.,0.));
#15473=DIRECTION('center_axis',(0.,-1.,0.));
#15474=DIRECTION('ref_axis',(0.,0.,-1.));
#15475=DIRECTION('center_axis',(0.,-1.,0.));
#15476=DIRECTION('ref_axis',(1.,0.,0.));
#15477=DIRECTION('center_axis',(0.,-1.,0.));
#15478=DIRECTION('ref_axis',(1.,0.,0.));
#15479=DIRECTION('center_axis',(1.,0.,1.22464679914735E-16));
#15480=DIRECTION('ref_axis',(-1.22464679914735E-16,0.,1.));
#15481=DIRECTION('center_axis',(0.,1.,0.));
#15482=DIRECTION('ref_axis',(1.,0.,0.));
#15483=DIRECTION('center_axis',(0.,1.,0.));
#15484=DIRECTION('ref_axis',(1.,0.,0.));
#15485=DIRECTION('center_axis',(0.,-1.,0.));
#15486=DIRECTION('ref_axis',(1.,0.,0.));
#15487=DIRECTION('center_axis',(0.,-1.,0.));
#15488=DIRECTION('ref_axis',(1.,0.,0.));
#15489=DIRECTION('',(0.,1.,0.));
#15490=DIRECTION('center_axis',(0.,1.,0.));
#15491=DIRECTION('ref_axis',(0.,0.,1.));
#15492=DIRECTION('center_axis',(0.,-1.,0.));
#15493=DIRECTION('ref_axis',(1.,0.,0.));
#15494=DIRECTION('center_axis',(0.,-1.,0.));
#15495=DIRECTION('ref_axis',(1.,0.,0.));
#15496=DIRECTION('center_axis',(0.,-1.,0.));
#15497=DIRECTION('ref_axis',(1.,0.,0.));
#15498=DIRECTION('center_axis',(0.,-1.,0.));
#15499=DIRECTION('ref_axis',(1.,0.,0.));
#15500=DIRECTION('',(0.707106781186548,0.707106781186547,8.65956056235494E-17));
#15501=DIRECTION('center_axis',(0.,-1.,0.));
#15502=DIRECTION('ref_axis',(1.,0.,0.));
#15503=DIRECTION('center_axis',(0.,-1.,0.));
#15504=DIRECTION('ref_axis',(1.,0.,0.));
#15505=DIRECTION('',(0.,1.,0.));
#15506=DIRECTION('center_axis',(0.,1.,0.));
#15507=DIRECTION('ref_axis',(1.,0.,0.));
#15508=DIRECTION('center_axis',(0.,-1.,0.));
#15509=DIRECTION('ref_axis',(1.,0.,0.));
#15510=DIRECTION('',(-0.707106781186548,0.707106781186547,-8.65956056235494E-17));
#15511=DIRECTION('center_axis',(0.,-1.,0.));
#15512=DIRECTION('ref_axis',(0.,0.,-1.));
#15513=DIRECTION('center_axis',(0.,-1.,0.));
#15514=DIRECTION('ref_axis',(1.,0.,0.));
#15515=DIRECTION('',(0.,1.,0.));
#15516=DIRECTION('axis',(0.,0.,1.));
#15517=DIRECTION('refdir',(1.,0.,0.));
#15518=DIRECTION('center_axis',(0.,0.,1.));
#15519=DIRECTION('ref_axis',(1.,0.,0.));
#15520=DIRECTION('center_axis',(1.22464679914735E-16,-1.,0.));
#15521=DIRECTION('ref_axis',(-1.,-1.22464679914735E-16,0.));
#15522=DIRECTION('center_axis',(0.707106781186548,0.,0.707106781186548));
#15523=DIRECTION('ref_axis',(0.707106781186548,0.,-0.707106781186548));
#15524=DIRECTION('center_axis',(8.65956056235494E-17,-1.,-8.65956056235493E-17));
#15525=DIRECTION('ref_axis',(-0.707106781186547,-1.22464679914735E-16,0.707106781186547));
#15526=DIRECTION('center_axis',(1.,0.,0.));
#15527=DIRECTION('ref_axis',(6.12323399573676E-17,0.,-1.));
#15528=DIRECTION('center_axis',(7.49879891330929E-33,-1.,-1.22464679914735E-16));
#15529=DIRECTION('ref_axis',(-6.12323399573676E-17,-1.22464679914735E-16,
1.));
#15530=DIRECTION('center_axis',(0.707106781186548,0.,-0.707106781186548));
#15531=DIRECTION('ref_axis',(-0.707106781186548,0.,-0.707106781186548));
#15532=DIRECTION('center_axis',(-8.65956056235493E-17,-1.,-8.65956056235494E-17));
#15533=DIRECTION('ref_axis',(0.707106781186547,-1.22464679914735E-16,0.707106781186547));
#15534=DIRECTION('center_axis',(0.,0.,-1.));
#15535=DIRECTION('ref_axis',(-1.,0.,-1.22464679914735E-16));
#15536=DIRECTION('center_axis',(-1.22464679914735E-16,-1.,-1.49975978266186E-32));
#15537=DIRECTION('ref_axis',(1.,-1.22464679914735E-16,1.22464679914735E-16));
#15538=DIRECTION('center_axis',(-0.707106781186547,0.,-0.707106781186548));
#15539=DIRECTION('ref_axis',(-0.707106781186548,0.,0.707106781186547));
#15540=DIRECTION('center_axis',(-8.65956056235493E-17,-1.,8.65956056235493E-17));
#15541=DIRECTION('ref_axis',(0.707106781186548,-1.22464679914735E-16,-0.707106781186547));
#15542=DIRECTION('center_axis',(-1.,0.,0.));
#15543=DIRECTION('ref_axis',(-1.83697019872103E-16,0.,1.));
#15544=DIRECTION('center_axis',(-2.24963967399279E-32,-1.,1.22464679914735E-16));
#15545=DIRECTION('ref_axis',(1.83697019872103E-16,-1.22464679914735E-16,
-1.));
#15546=DIRECTION('center_axis',(-0.707106781186548,0.,0.707106781186548));
#15547=DIRECTION('ref_axis',(0.707106781186547,0.,0.707106781186548));
#15548=DIRECTION('center_axis',(8.65956056235493E-17,-1.,8.65956056235493E-17));
#15549=DIRECTION('ref_axis',(-0.707106781186547,-1.22464679914735E-16,-0.707106781186548));
#15550=DIRECTION('axis',(0.,0.,1.));
#15551=DIRECTION('refdir',(1.,0.,0.));
#15552=DIRECTION('center_axis',(0.,0.,1.));
#15553=DIRECTION('ref_axis',(1.,0.,0.));
#15554=DIRECTION('center_axis',(0.,-1.,0.));
#15555=DIRECTION('ref_axis',(0.,0.,-1.));
#15556=DIRECTION('center_axis',(0.,-1.,0.));
#15557=DIRECTION('ref_axis',(0.,0.,-1.));
#15558=DIRECTION('center_axis',(0.,1.,0.));
#15559=DIRECTION('ref_axis',(1.,0.,0.));
#15560=DIRECTION('center_axis',(0.,1.,0.));
#15561=DIRECTION('ref_axis',(1.,0.,0.));
#15562=DIRECTION('center_axis',(0.,1.,0.));
#15563=DIRECTION('ref_axis',(1.,0.,0.));
#15564=DIRECTION('center_axis',(0.,1.,0.));
#15565=DIRECTION('ref_axis',(1.,0.,0.));
#15566=DIRECTION('',(0.,-1.,0.));
#15567=DIRECTION('center_axis',(0.,-1.,0.));
#15568=DIRECTION('ref_axis',(1.,0.,0.));
#15569=DIRECTION('center_axis',(0.,1.,0.));
#15570=DIRECTION('ref_axis',(1.,0.,0.));
#15571=DIRECTION('center_axis',(0.,1.,0.));
#15572=DIRECTION('ref_axis',(1.,0.,0.));
#15573=DIRECTION('center_axis',(0.,1.,0.));
#15574=DIRECTION('ref_axis',(1.,0.,0.));
#15575=DIRECTION('center_axis',(0.,1.,0.));
#15576=DIRECTION('ref_axis',(1.,0.,0.));
#15577=DIRECTION('center_axis',(0.,1.,0.));
#15578=DIRECTION('ref_axis',(1.,0.,0.));
#15579=DIRECTION('center_axis',(0.,1.,0.));
#15580=DIRECTION('ref_axis',(1.,0.,0.));
#15581=DIRECTION('center_axis',(0.,-1.,0.));
#15582=DIRECTION('ref_axis',(1.,0.,0.));
#15583=DIRECTION('center_axis',(0.,-1.,0.));
#15584=DIRECTION('ref_axis',(0.,0.,-1.));
#15585=DIRECTION('center_axis',(6.12323399573677E-17,0.,1.));
#15586=DIRECTION('ref_axis',(1.,0.,0.));
#15587=DIRECTION('center_axis',(0.,-1.,0.));
#15588=DIRECTION('ref_axis',(0.,0.,-1.));
#15589=DIRECTION('center_axis',(0.,1.,0.));
#15590=DIRECTION('ref_axis',(1.,0.,0.));
#15591=DIRECTION('center_axis',(0.,-1.,0.));
#15592=DIRECTION('ref_axis',(1.,0.,0.));
#15593=DIRECTION('center_axis',(0.,-1.,0.));
#15594=DIRECTION('ref_axis',(0.,0.,-1.));
#15595=DIRECTION('center_axis',(0.,0.,1.));
#15596=DIRECTION('ref_axis',(1.,0.,0.));
#15597=DIRECTION('center_axis',(0.,-1.,0.));
#15598=DIRECTION('ref_axis',(0.,0.,-1.));
#15599=DIRECTION('center_axis',(0.,1.,0.));
#15600=DIRECTION('ref_axis',(1.,0.,0.));
#15601=DIRECTION('center_axis',(0.,-1.,0.));
#15602=DIRECTION('ref_axis',(1.,0.,0.));
#15603=DIRECTION('center_axis',(0.,-1.,0.));
#15604=DIRECTION('ref_axis',(0.,0.,-1.));
#15605=DIRECTION('center_axis',(0.,0.,1.));
#15606=DIRECTION('ref_axis',(1.,0.,0.));
#15607=DIRECTION('center_axis',(0.,-1.,0.));
#15608=DIRECTION('ref_axis',(0.,0.,-1.));
#15609=DIRECTION('center_axis',(0.,1.,0.));
#15610=DIRECTION('ref_axis',(1.,0.,0.));
#15611=DIRECTION('center_axis',(0.,-1.,0.));
#15612=DIRECTION('ref_axis',(1.,0.,0.));
#15613=DIRECTION('center_axis',(0.,-1.,0.));
#15614=DIRECTION('ref_axis',(0.,0.,-1.));
#15615=DIRECTION('center_axis',(0.,0.,1.));
#15616=DIRECTION('ref_axis',(1.,0.,0.));
#15617=DIRECTION('center_axis',(0.,-1.,0.));
#15618=DIRECTION('ref_axis',(0.,0.,-1.));
#15619=DIRECTION('center_axis',(0.,1.,0.));
#15620=DIRECTION('ref_axis',(1.,0.,0.));
#15621=DIRECTION('center_axis',(0.,-1.,0.));
#15622=DIRECTION('ref_axis',(1.,0.,0.));
#15623=DIRECTION('center_axis',(0.,-1.,0.));
#15624=DIRECTION('ref_axis',(0.,0.,-1.));
#15625=DIRECTION('center_axis',(6.12323399573676E-17,0.,1.));
#15626=DIRECTION('ref_axis',(1.,0.,0.));
#15627=DIRECTION('center_axis',(0.,-1.,0.));
#15628=DIRECTION('ref_axis',(0.,0.,-1.));
#15629=DIRECTION('center_axis',(0.,1.,0.));
#15630=DIRECTION('ref_axis',(1.,0.,0.));
#15631=DIRECTION('center_axis',(0.,-1.,0.));
#15632=DIRECTION('ref_axis',(1.,0.,0.));
#15633=DIRECTION('center_axis',(0.,-1.,0.));
#15634=DIRECTION('ref_axis',(0.,0.,-1.));
#15635=DIRECTION('center_axis',(0.,0.,1.));
#15636=DIRECTION('ref_axis',(1.,0.,0.));
#15637=DIRECTION('center_axis',(0.,-1.,0.));
#15638=DIRECTION('ref_axis',(0.,0.,-1.));
#15639=DIRECTION('center_axis',(0.,1.,0.));
#15640=DIRECTION('ref_axis',(1.,0.,0.));
#15641=DIRECTION('center_axis',(0.,1.,0.));
#15642=DIRECTION('ref_axis',(1.,0.,0.));
#15643=DIRECTION('',(0.,1.,0.));
#15644=DIRECTION('center_axis',(0.,-1.,0.));
#15645=DIRECTION('ref_axis',(1.,0.,0.));
#15646=DIRECTION('center_axis',(0.,-1.,0.));
#15647=DIRECTION('ref_axis',(1.,0.,0.));
#15648=DIRECTION('center_axis',(0.,1.,0.));
#15649=DIRECTION('ref_axis',(1.,0.,0.));
#15650=DIRECTION('center_axis',(0.,-1.,0.));
#15651=DIRECTION('ref_axis',(0.,0.,-1.));
#15652=DIRECTION('center_axis',(0.,0.,1.));
#15653=DIRECTION('ref_axis',(1.,0.,0.));
#15654=DIRECTION('center_axis',(0.,-1.,0.));
#15655=DIRECTION('ref_axis',(0.,0.,-1.));
#15656=DIRECTION('center_axis',(0.,-1.,0.));
#15657=DIRECTION('ref_axis',(-1.,0.,0.));
#15658=DIRECTION('center_axis',(0.,1.,0.));
#15659=DIRECTION('ref_axis',(1.,0.,0.));
#15660=DIRECTION('axis',(0.,0.,1.));
#15661=DIRECTION('refdir',(1.,0.,0.));
#15662=DIRECTION('center_axis',(0.,1.,0.));
#15663=DIRECTION('ref_axis',(0.,0.,1.));
#15664=DIRECTION('center_axis',(0.,-1.,0.));
#15665=DIRECTION('ref_axis',(1.,0.,0.));
#15666=DIRECTION('center_axis',(0.,-1.,0.));
#15667=DIRECTION('ref_axis',(1.,0.,0.));
#15668=DIRECTION('center_axis',(0.,-1.,0.));
#15669=DIRECTION('ref_axis',(1.,0.,0.));
#15670=DIRECTION('center_axis',(0.,-1.,0.));
#15671=DIRECTION('ref_axis',(1.,0.,0.));
#15672=DIRECTION('',(0.,1.,0.));
#15673=DIRECTION('center_axis',(0.,-1.,0.));
#15674=DIRECTION('ref_axis',(0.,0.,-1.));
#15675=DIRECTION('center_axis',(0.,-1.,0.));
#15676=DIRECTION('ref_axis',(1.,0.,0.));
#15677=DIRECTION('center_axis',(0.,-1.,0.));
#15678=DIRECTION('ref_axis',(1.,0.,0.));
#15679=DIRECTION('',(0.,1.,0.));
#15680=DIRECTION('center_axis',(0.,1.,0.));
#15681=DIRECTION('ref_axis',(0.,0.,1.));
#15682=DIRECTION('center_axis',(0.,-1.,0.));
#15683=DIRECTION('ref_axis',(1.,0.,0.));
#15684=DIRECTION('center_axis',(0.,-1.,0.));
#15685=DIRECTION('ref_axis',(1.,0.,0.));
#15686=DIRECTION('center_axis',(0.,-1.,0.));
#15687=DIRECTION('ref_axis',(1.,0.,0.));
#15688=DIRECTION('center_axis',(0.,-1.,0.));
#15689=DIRECTION('ref_axis',(1.,0.,0.));
#15690=DIRECTION('',(0.,1.,0.));
#15691=DIRECTION('center_axis',(0.,-1.,0.));
#15692=DIRECTION('ref_axis',(0.,0.,-1.));
#15693=DIRECTION('center_axis',(0.,-1.,0.));
#15694=DIRECTION('ref_axis',(1.,0.,0.));
#15695=DIRECTION('center_axis',(0.,-1.,0.));
#15696=DIRECTION('ref_axis',(1.,0.,0.));
#15697=DIRECTION('',(0.,1.,0.));
#15698=DIRECTION('',(0.,0.,1.));
#15699=DIRECTION('',(1.,0.,0.));
#15700=DIRECTION('',(0.,0.,1.));
#15701=DIRECTION('',(1.,0.,0.));
#15702=DIRECTION('',(0.,0.,1.));
#15703=DIRECTION('',(1.,0.,0.));
#15704=DIRECTION('',(0.,0.,1.));
#15705=DIRECTION('',(1.,0.,0.));
#15706=DIRECTION('',(0.,0.,1.));
#15707=DIRECTION('',(1.,0.,0.));
#15708=DIRECTION('axis',(0.,0.,1.));
#15709=DIRECTION('refdir',(1.,0.,0.));
#15710=DIRECTION('axis',(0.,0.,1.));
#15711=DIRECTION('refdir',(1.,0.,0.));
#15712=DIRECTION('center_axis',(0.,0.,1.));
#15713=DIRECTION('ref_axis',(1.,0.,0.));
#15714=DIRECTION('center_axis',(0.,0.,1.));
#15715=DIRECTION('ref_axis',(1.,0.,0.));
#15716=DIRECTION('',(0.,0.,1.));
#15717=DIRECTION('center_axis',(0.,0.,-1.));
#15718=DIRECTION('ref_axis',(1.,0.,0.));
#15719=DIRECTION('center_axis',(0.,0.,1.));
#15720=DIRECTION('ref_axis',(1.,0.,0.));
#15721=DIRECTION('center_axis',(0.,0.,1.));
#15722=DIRECTION('ref_axis',(1.,0.,0.));
#15723=DIRECTION('',(0.,0.,1.));
#15724=DIRECTION('center_axis',(0.,0.,-1.));
#15725=DIRECTION('ref_axis',(1.,0.,0.));
#15726=DIRECTION('center_axis',(0.,0.,1.));
#15727=DIRECTION('ref_axis',(1.,0.,0.));
#15728=DIRECTION('center_axis',(0.,0.,1.));
#15729=DIRECTION('ref_axis',(1.,0.,0.));
#15730=DIRECTION('',(0.,0.,1.));
#15731=DIRECTION('center_axis',(0.,0.,-1.));
#15732=DIRECTION('ref_axis',(1.,0.,0.));
#15733=DIRECTION('center_axis',(0.,0.,1.));
#15734=DIRECTION('ref_axis',(1.,0.,0.));
#15735=DIRECTION('center_axis',(0.,0.,1.));
#15736=DIRECTION('ref_axis',(1.,0.,0.));
#15737=DIRECTION('',(0.,0.,1.));
#15738=DIRECTION('center_axis',(0.,0.,-1.));
#15739=DIRECTION('ref_axis',(1.,0.,0.));
#15740=DIRECTION('center_axis',(0.,0.,1.));
#15741=DIRECTION('ref_axis',(1.,0.,0.));
#15742=DIRECTION('center_axis',(0.,0.,1.));
#15743=DIRECTION('ref_axis',(1.,0.,0.));
#15744=DIRECTION('',(0.,0.,1.));
#15745=DIRECTION('center_axis',(0.,0.,-1.));
#15746=DIRECTION('ref_axis',(1.,0.,0.));
#15747=DIRECTION('center_axis',(0.,0.,1.));
#15748=DIRECTION('ref_axis',(1.,0.,0.));
#15749=DIRECTION('center_axis',(0.,0.,1.));
#15750=DIRECTION('ref_axis',(1.,0.,0.));
#15751=DIRECTION('',(0.,0.,1.));
#15752=DIRECTION('center_axis',(0.,0.,-1.));
#15753=DIRECTION('ref_axis',(1.,0.,0.));
#15754=DIRECTION('center_axis',(0.,0.,1.));
#15755=DIRECTION('ref_axis',(1.,0.,0.));
#15756=DIRECTION('center_axis',(0.,0.,1.));
#15757=DIRECTION('ref_axis',(1.,0.,0.));
#15758=DIRECTION('',(0.,0.,1.));
#15759=DIRECTION('center_axis',(0.,0.,-1.));
#15760=DIRECTION('ref_axis',(1.,0.,0.));
#15761=DIRECTION('center_axis',(0.,0.,1.));
#15762=DIRECTION('ref_axis',(1.,0.,0.));
#15763=DIRECTION('center_axis',(0.,0.,1.));
#15764=DIRECTION('ref_axis',(1.,0.,0.));
#15765=DIRECTION('',(0.,0.,1.));
#15766=DIRECTION('center_axis',(0.,0.,-1.));
#15767=DIRECTION('ref_axis',(1.,0.,0.));
#15768=DIRECTION('center_axis',(0.,0.,1.));
#15769=DIRECTION('ref_axis',(1.,0.,0.));
#15770=DIRECTION('center_axis',(0.,0.,1.));
#15771=DIRECTION('ref_axis',(1.,0.,0.));
#15772=DIRECTION('',(0.,0.,1.));
#15773=DIRECTION('center_axis',(0.,0.,-1.));
#15774=DIRECTION('ref_axis',(1.,0.,0.));
#15775=DIRECTION('center_axis',(0.,0.,1.));
#15776=DIRECTION('ref_axis',(1.,0.,0.));
#15777=DIRECTION('center_axis',(0.,0.,1.));
#15778=DIRECTION('ref_axis',(1.,0.,0.));
#15779=DIRECTION('',(0.,0.,1.));
#15780=DIRECTION('center_axis',(0.,0.,-1.));
#15781=DIRECTION('ref_axis',(1.,0.,0.));
#15782=DIRECTION('center_axis',(0.,1.,0.));
#15783=DIRECTION('ref_axis',(-1.,0.,0.));
#15784=DIRECTION('',(-1.,0.,0.));
#15785=DIRECTION('',(0.,0.,1.));
#15786=DIRECTION('',(-1.,0.,0.));
#15787=DIRECTION('',(0.,0.,1.));
#15788=DIRECTION('center_axis',(1.,0.,0.));
#15789=DIRECTION('ref_axis',(0.,1.,0.));
#15790=DIRECTION('',(0.,1.,0.));
#15791=DIRECTION('',(0.,1.,0.));
#15792=DIRECTION('',(0.,0.,1.));
#15793=DIRECTION('center_axis',(0.,-1.,0.));
#15794=DIRECTION('ref_axis',(1.,0.,0.));
#15795=DIRECTION('',(1.,0.,0.));
#15796=DIRECTION('',(1.,0.,0.));
#15797=DIRECTION('',(0.,0.,1.));
#15798=DIRECTION('center_axis',(-1.,0.,0.));
#15799=DIRECTION('ref_axis',(0.,-1.,0.));
#15800=DIRECTION('',(0.,-1.,0.));
#15801=DIRECTION('',(0.,-1.,0.));
#15802=DIRECTION('center_axis',(0.,0.,1.));
#15803=DIRECTION('ref_axis',(1.,0.,0.));
#15804=DIRECTION('center_axis',(0.,0.,1.));
#15805=DIRECTION('ref_axis',(1.,0.,0.));
#15806=DIRECTION('axis',(0.,0.,1.));
#15807=DIRECTION('refdir',(1.,0.,0.));
#15808=DIRECTION('center_axis',(0.,1.,0.));
#15809=DIRECTION('ref_axis',(1.,0.,0.));
#15810=DIRECTION('center_axis',(0.,1.,0.));
#15811=DIRECTION('ref_axis',(1.,0.,0.));
#15812=DIRECTION('',(0.,1.,0.));
#15813=DIRECTION('center_axis',(0.,-1.,0.));
#15814=DIRECTION('ref_axis',(1.,0.,0.));
#15815=DIRECTION('center_axis',(0.,1.,0.));
#15816=DIRECTION('ref_axis',(1.,0.,0.));
#15817=DIRECTION('center_axis',(0.,1.,0.));
#15818=DIRECTION('ref_axis',(1.,0.,0.));
#15819=DIRECTION('',(0.,1.,0.));
#15820=DIRECTION('center_axis',(0.,-1.,0.));
#15821=DIRECTION('ref_axis',(1.,0.,0.));
#15822=DIRECTION('center_axis',(0.,1.,0.));
#15823=DIRECTION('ref_axis',(1.,0.,0.));
#15824=DIRECTION('center_axis',(0.,1.,0.));
#15825=DIRECTION('ref_axis',(1.,0.,0.));
#15826=DIRECTION('',(0.,1.,0.));
#15827=DIRECTION('center_axis',(0.,-1.,0.));
#15828=DIRECTION('ref_axis',(1.,0.,0.));
#15829=DIRECTION('center_axis',(0.,1.,0.));
#15830=DIRECTION('ref_axis',(1.,0.,0.));
#15831=DIRECTION('center_axis',(0.,1.,0.));
#15832=DIRECTION('ref_axis',(1.,0.,0.));
#15833=DIRECTION('',(0.,1.,0.));
#15834=DIRECTION('center_axis',(0.,-1.,0.));
#15835=DIRECTION('ref_axis',(1.,0.,0.));
#15836=DIRECTION('center_axis',(0.,1.,0.));
#15837=DIRECTION('ref_axis',(1.,0.,0.));
#15838=DIRECTION('center_axis',(0.,1.,0.));
#15839=DIRECTION('ref_axis',(1.,0.,0.));
#15840=DIRECTION('',(0.,1.,0.));
#15841=DIRECTION('center_axis',(0.,-1.,0.));
#15842=DIRECTION('ref_axis',(1.,0.,0.));
#15843=DIRECTION('center_axis',(0.,0.,1.));
#15844=DIRECTION('ref_axis',(1.,0.,0.));
#15845=DIRECTION('',(1.,0.,0.));
#15846=DIRECTION('center_axis',(0.,0.,1.));
#15847=DIRECTION('ref_axis',(1.,0.,0.));
#15848=DIRECTION('center_axis',(0.,0.,1.));
#15849=DIRECTION('ref_axis',(1.,0.,0.));
#15850=DIRECTION('',(0.,0.,1.));
#15851=DIRECTION('center_axis',(0.,0.,1.));
#15852=DIRECTION('ref_axis',(1.,0.,0.));
#15853=DIRECTION('',(0.,0.,-1.));
#15854=DIRECTION('center_axis',(0.,0.,1.));
#15855=DIRECTION('ref_axis',(1.,0.,0.));
#15856=DIRECTION('',(-1.,0.,0.));
#15857=DIRECTION('center_axis',(0.,0.,1.));
#15858=DIRECTION('ref_axis',(1.,0.,0.));
#15859=DIRECTION('center_axis',(0.,0.,1.));
#15860=DIRECTION('ref_axis',(1.,0.,0.));
#15861=DIRECTION('',(0.,0.,1.));
#15862=DIRECTION('center_axis',(0.,0.,1.));
#15863=DIRECTION('ref_axis',(1.,0.,0.));
#15864=DIRECTION('',(0.,0.,-1.));
#15865=DIRECTION('center_axis',(0.,0.,1.));
#15866=DIRECTION('ref_axis',(1.,0.,0.));
#15867=DIRECTION('',(1.,0.,0.));
#15868=DIRECTION('center_axis',(0.,0.,1.));
#15869=DIRECTION('ref_axis',(1.,0.,0.));
#15870=DIRECTION('center_axis',(0.,0.,1.));
#15871=DIRECTION('ref_axis',(1.,0.,0.));
#15872=DIRECTION('',(0.,0.,1.));
#15873=DIRECTION('center_axis',(0.,0.,1.));
#15874=DIRECTION('ref_axis',(1.,0.,0.));
#15875=DIRECTION('',(0.,0.,-1.));
#15876=DIRECTION('center_axis',(0.,0.,1.));
#15877=DIRECTION('ref_axis',(1.,0.,0.));
#15878=DIRECTION('',(-1.,0.,0.));
#15879=DIRECTION('center_axis',(0.,0.,1.));
#15880=DIRECTION('ref_axis',(1.,0.,0.));
#15881=DIRECTION('center_axis',(0.,0.,1.));
#15882=DIRECTION('ref_axis',(1.,0.,0.));
#15883=DIRECTION('',(0.,0.,1.));
#15884=DIRECTION('center_axis',(0.,0.,1.));
#15885=DIRECTION('ref_axis',(1.,0.,0.));
#15886=DIRECTION('',(0.,0.,-1.));
#15887=DIRECTION('center_axis',(0.,-1.,0.));
#15888=DIRECTION('ref_axis',(1.,0.,0.));
#15889=DIRECTION('',(1.,0.,0.));
#15890=DIRECTION('',(0.,0.,1.));
#15891=DIRECTION('',(-1.,0.,0.));
#15892=DIRECTION('',(0.,0.,1.));
#15893=DIRECTION('',(1.,0.,0.));
#15894=DIRECTION('',(0.,0.,1.));
#15895=DIRECTION('',(-1.,0.,0.));
#15896=DIRECTION('',(0.,0.,-1.));
#15897=DIRECTION('',(1.,0.,0.));
#15898=DIRECTION('',(1.,0.,0.));
#15899=DIRECTION('center_axis',(0.,1.,0.));
#15900=DIRECTION('ref_axis',(-1.,0.,0.));
#15901=DIRECTION('',(-1.,0.,0.));
#15902=DIRECTION('',(0.,0.,1.));
#15903=DIRECTION('',(1.,0.,0.));
#15904=DIRECTION('',(0.,0.,1.));
#15905=DIRECTION('',(-1.,0.,0.));
#15906=DIRECTION('',(0.,0.,1.));
#15907=DIRECTION('',(1.,0.,0.));
#15908=DIRECTION('',(0.,0.,-1.));
#15909=DIRECTION('',(-1.,0.,0.));
#15910=DIRECTION('',(-1.,0.,0.));
#15911=DIRECTION('center_axis',(0.,0.,1.));
#15912=DIRECTION('ref_axis',(1.,0.,0.));
#15913=DIRECTION('center_axis',(0.,0.,1.));
#15914=DIRECTION('ref_axis',(1.,0.,0.));
#15915=DIRECTION('',(0.,0.,1.));
#15916=DIRECTION('center_axis',(0.,0.,-1.));
#15917=DIRECTION('ref_axis',(1.,0.,0.));
#15918=DIRECTION('center_axis',(0.,0.,1.));
#15919=DIRECTION('ref_axis',(1.,0.,0.));
#15920=DIRECTION('center_axis',(0.,0.,1.));
#15921=DIRECTION('ref_axis',(1.,0.,0.));
#15922=DIRECTION('',(0.,0.,1.));
#15923=DIRECTION('center_axis',(0.,0.,-1.));
#15924=DIRECTION('ref_axis',(1.,0.,0.));
#15925=DIRECTION('center_axis',(0.,0.,1.));
#15926=DIRECTION('ref_axis',(1.,0.,0.));
#15927=DIRECTION('center_axis',(0.,0.,1.));
#15928=DIRECTION('ref_axis',(1.,0.,0.));
#15929=DIRECTION('',(0.,0.,1.));
#15930=DIRECTION('center_axis',(0.,0.,-1.));
#15931=DIRECTION('ref_axis',(1.,0.,0.));
#15932=DIRECTION('center_axis',(0.,0.,1.));
#15933=DIRECTION('ref_axis',(1.,0.,0.));
#15934=DIRECTION('center_axis',(0.,0.,1.));
#15935=DIRECTION('ref_axis',(1.,0.,0.));
#15936=DIRECTION('',(0.,0.,1.));
#15937=DIRECTION('center_axis',(0.,0.,-1.));
#15938=DIRECTION('ref_axis',(1.,0.,0.));
#15939=DIRECTION('center_axis',(0.,0.,1.));
#15940=DIRECTION('ref_axis',(1.,0.,0.));
#15941=DIRECTION('',(0.,1.,0.));
#15942=DIRECTION('',(0.,1.,0.));
#15943=DIRECTION('center_axis',(0.,0.,1.));
#15944=DIRECTION('ref_axis',(1.,0.,0.));
#15945=DIRECTION('',(0.,-1.,0.));
#15946=DIRECTION('',(0.,1.,0.));
#15947=DIRECTION('center_axis',(-1.,0.,0.));
#15948=DIRECTION('ref_axis',(0.,0.,1.));
#15949=DIRECTION('',(0.,1.,0.));
#15950=DIRECTION('center_axis',(1.,0.,0.));
#15951=DIRECTION('ref_axis',(0.,0.,-1.));
#15952=DIRECTION('',(0.,1.,0.));
#15953=DIRECTION('center_axis',(1.,0.,0.));
#15954=DIRECTION('ref_axis',(0.,1.,0.));
#15955=DIRECTION('',(0.,1.,0.));
#15956=DIRECTION('center_axis',(-1.,0.,0.));
#15957=DIRECTION('ref_axis',(0.,-1.,0.));
#15958=DIRECTION('',(0.,-1.,0.));
#15959=DIRECTION('center_axis',(0.,0.,1.));
#15960=DIRECTION('ref_axis',(1.,0.,0.));
#15961=DIRECTION('center_axis',(0.,0.,1.));
#15962=DIRECTION('ref_axis',(1.,0.,0.));
#15963=DIRECTION('axis',(0.,0.,1.));
#15964=DIRECTION('refdir',(1.,0.,0.));
#15965=DIRECTION('center_axis',(0.,1.,0.));
#15966=DIRECTION('ref_axis',(1.,0.,0.));
#15967=DIRECTION('center_axis',(0.,-1.,0.));
#15968=DIRECTION('ref_axis',(1.,0.,0.));
#15969=DIRECTION('',(0.,-1.,0.));
#15970=DIRECTION('center_axis',(0.,-1.,0.));
#15971=DIRECTION('ref_axis',(1.,0.,0.));
#15972=DIRECTION('center_axis',(0.,1.,0.));
#15973=DIRECTION('ref_axis',(1.,0.,0.));
#15974=DIRECTION('center_axis',(0.,1.,0.));
#15975=DIRECTION('ref_axis',(1.,0.,0.));
#15976=DIRECTION('',(0.,-1.,0.));
#15977=DIRECTION('center_axis',(0.,1.,0.));
#15978=DIRECTION('ref_axis',(1.,0.,0.));
#15979=DIRECTION('center_axis',(0.,1.,0.));
#15980=DIRECTION('ref_axis',(1.,0.,0.));
#15981=DIRECTION('center_axis',(0.,1.,0.));
#15982=DIRECTION('ref_axis',(1.,0.,0.));
#15983=DIRECTION('axis',(0.,0.,1.));
#15984=DIRECTION('refdir',(1.,0.,0.));
#15985=DIRECTION('center_axis',(0.,1.,0.));
#15986=DIRECTION('ref_axis',(0.707106781186549,0.,0.707106781186546));
#15987=DIRECTION('',(0.,1.,0.));
#15988=DIRECTION('center_axis',(0.,1.,0.));
#15989=DIRECTION('ref_axis',(1.,0.,0.));
#15990=DIRECTION('',(0.,-1.,0.));
#15991=DIRECTION('center_axis',(0.,-1.,0.));
#15992=DIRECTION('ref_axis',(1.,0.,0.));
#15993=DIRECTION('center_axis',(0.,1.,0.));
#15994=DIRECTION('ref_axis',(0.707106781186547,0.,-0.707106781186548));
#15995=DIRECTION('',(0.,1.,0.));
#15996=DIRECTION('center_axis',(0.,1.,0.));
#15997=DIRECTION('ref_axis',(1.,0.,0.));
#15998=DIRECTION('',(0.,-1.,0.));
#15999=DIRECTION('center_axis',(0.,-1.,0.));
#16000=DIRECTION('ref_axis',(1.,0.,0.));
#16001=DIRECTION('center_axis',(0.,1.,0.));
#16002=DIRECTION('ref_axis',(-0.707106781186548,0.,-0.707106781186547));
#16003=DIRECTION('',(0.,1.,0.));
#16004=DIRECTION('center_axis',(0.,1.,0.));
#16005=DIRECTION('ref_axis',(1.,0.,0.));
#16006=DIRECTION('',(0.,-1.,0.));
#16007=DIRECTION('center_axis',(0.,-1.,0.));
#16008=DIRECTION('ref_axis',(1.,0.,0.));
#16009=DIRECTION('center_axis',(0.,1.,0.));
#16010=DIRECTION('ref_axis',(-0.707106781186552,0.,0.707106781186543));
#16011=DIRECTION('',(0.,1.,0.));
#16012=DIRECTION('center_axis',(0.,1.,0.));
#16013=DIRECTION('ref_axis',(1.,0.,0.));
#16014=DIRECTION('',(0.,-1.,0.));
#16015=DIRECTION('center_axis',(0.,-1.,0.));
#16016=DIRECTION('ref_axis',(1.,0.,0.));
#16017=DIRECTION('center_axis',(0.,1.,0.));
#16018=DIRECTION('ref_axis',(1.,0.,0.));
#16019=DIRECTION('center_axis',(0.,1.,0.));
#16020=DIRECTION('ref_axis',(1.,0.,0.));
#16021=DIRECTION('center_axis',(0.,1.,0.));
#16022=DIRECTION('ref_axis',(1.,0.,0.));
#16023=DIRECTION('center_axis',(0.,1.,0.));
#16024=DIRECTION('ref_axis',(1.,0.,0.));
#16025=DIRECTION('center_axis',(0.,1.,0.));
#16026=DIRECTION('ref_axis',(1.,0.,0.));
#16027=DIRECTION('center_axis',(0.,-1.,0.));
#16028=DIRECTION('ref_axis',(1.,0.,0.));
#16029=DIRECTION('center_axis',(0.,1.,0.));
#16030=DIRECTION('ref_axis',(1.,0.,0.));
#16031=DIRECTION('center_axis',(0.,1.,0.));
#16032=DIRECTION('ref_axis',(1.,0.,0.));
#16033=DIRECTION('center_axis',(0.,1.,0.));
#16034=DIRECTION('ref_axis',(1.,0.,0.));
#16035=DIRECTION('center_axis',(0.,1.,0.));
#16036=DIRECTION('ref_axis',(1.,0.,0.));
#16037=DIRECTION('center_axis',(0.,1.,0.));
#16038=DIRECTION('ref_axis',(1.,0.,0.));
#16039=DIRECTION('center_axis',(0.,1.,0.));
#16040=DIRECTION('ref_axis',(1.,0.,0.));
#16041=DIRECTION('center_axis',(0.,1.,0.));
#16042=DIRECTION('ref_axis',(-1.,0.,-1.22464679914735E-16));
#16043=DIRECTION('center_axis',(0.,1.,0.));
#16044=DIRECTION('ref_axis',(1.,0.,0.));
#16045=DIRECTION('center_axis',(0.,1.,0.));
#16046=DIRECTION('ref_axis',(1.,0.,0.));
#16047=DIRECTION('center_axis',(0.,1.,0.));
#16048=DIRECTION('ref_axis',(1.,0.,0.));
#16049=DIRECTION('',(0.,-1.,0.));
#16050=DIRECTION('center_axis',(0.,-1.,0.));
#16051=DIRECTION('ref_axis',(1.,0.,0.));
#16052=DIRECTION('center_axis',(0.,1.,0.));
#16053=DIRECTION('ref_axis',(1.,0.,0.));
#16054=DIRECTION('center_axis',(0.,-1.,0.));
#16055=DIRECTION('ref_axis',(1.,0.,0.));
#16056=DIRECTION('center_axis',(0.,1.,0.));
#16057=DIRECTION('ref_axis',(1.,0.,0.));
#16058=DIRECTION('',(0.,-1.,0.));
#16059=DIRECTION('center_axis',(0.,1.,0.));
#16060=DIRECTION('ref_axis',(1.,0.,0.));
#16061=DIRECTION('axis',(0.,0.,1.));
#16062=DIRECTION('refdir',(1.,0.,0.));
#16063=DIRECTION('center_axis',(0.,1.,0.));
#16064=DIRECTION('ref_axis',(0.707106781186549,0.,0.707106781186546));
#16065=DIRECTION('',(0.,1.,0.));
#16066=DIRECTION('center_axis',(0.,1.,0.));
#16067=DIRECTION('ref_axis',(1.,0.,0.));
#16068=DIRECTION('',(0.,-1.,0.));
#16069=DIRECTION('center_axis',(0.,-1.,0.));
#16070=DIRECTION('ref_axis',(1.,0.,0.));
#16071=DIRECTION('center_axis',(0.,1.,0.));
#16072=DIRECTION('ref_axis',(0.707106781186547,0.,-0.707106781186548));
#16073=DIRECTION('',(0.,1.,0.));
#16074=DIRECTION('center_axis',(0.,1.,0.));
#16075=DIRECTION('ref_axis',(1.,0.,0.));
#16076=DIRECTION('',(0.,-1.,0.));
#16077=DIRECTION('center_axis',(0.,-1.,0.));
#16078=DIRECTION('ref_axis',(1.,0.,0.));
#16079=DIRECTION('center_axis',(0.,1.,0.));
#16080=DIRECTION('ref_axis',(-0.707106781186548,0.,-0.707106781186547));
#16081=DIRECTION('',(0.,1.,0.));
#16082=DIRECTION('center_axis',(0.,1.,0.));
#16083=DIRECTION('ref_axis',(1.,0.,0.));
#16084=DIRECTION('',(0.,-1.,0.));
#16085=DIRECTION('center_axis',(0.,-1.,0.));
#16086=DIRECTION('ref_axis',(1.,0.,0.));
#16087=DIRECTION('center_axis',(0.,1.,0.));
#16088=DIRECTION('ref_axis',(-0.707106781186552,0.,0.707106781186543));
#16089=DIRECTION('',(0.,1.,0.));
#16090=DIRECTION('center_axis',(0.,1.,0.));
#16091=DIRECTION('ref_axis',(1.,0.,0.));
#16092=DIRECTION('',(0.,-1.,0.));
#16093=DIRECTION('center_axis',(0.,-1.,0.));
#16094=DIRECTION('ref_axis',(1.,0.,0.));
#16095=DIRECTION('center_axis',(0.,1.,0.));
#16096=DIRECTION('ref_axis',(1.,0.,0.));
#16097=DIRECTION('center_axis',(0.,1.,0.));
#16098=DIRECTION('ref_axis',(1.,0.,0.));
#16099=DIRECTION('center_axis',(0.,1.,0.));
#16100=DIRECTION('ref_axis',(1.,0.,0.));
#16101=DIRECTION('center_axis',(0.,1.,0.));
#16102=DIRECTION('ref_axis',(1.,0.,0.));
#16103=DIRECTION('center_axis',(0.,1.,0.));
#16104=DIRECTION('ref_axis',(1.,0.,0.));
#16105=DIRECTION('center_axis',(0.,1.,0.));
#16106=DIRECTION('ref_axis',(1.,0.,0.));
#16107=DIRECTION('center_axis',(0.,1.,0.));
#16108=DIRECTION('ref_axis',(1.,0.,0.));
#16109=DIRECTION('center_axis',(0.,1.,0.));
#16110=DIRECTION('ref_axis',(1.,0.,0.));
#16111=DIRECTION('center_axis',(0.,1.,0.));
#16112=DIRECTION('ref_axis',(1.,0.,0.));
#16113=DIRECTION('center_axis',(0.,1.,0.));
#16114=DIRECTION('ref_axis',(1.,0.,0.));
#16115=DIRECTION('center_axis',(0.,1.,0.));
#16116=DIRECTION('ref_axis',(1.,0.,0.));
#16117=DIRECTION('center_axis',(0.,1.,0.));
#16118=DIRECTION('ref_axis',(1.,0.,0.));
#16119=DIRECTION('center_axis',(0.,1.,0.));
#16120=DIRECTION('ref_axis',(-1.,0.,-1.22464679914735E-16));
#16121=DIRECTION('center_axis',(0.,1.,0.));
#16122=DIRECTION('ref_axis',(1.,0.,0.));
#16123=DIRECTION('center_axis',(0.,1.,0.));
#16124=DIRECTION('ref_axis',(1.,0.,0.));
#16125=DIRECTION('',(0.,-1.,0.));
#16126=DIRECTION('center_axis',(0.,1.,0.));
#16127=DIRECTION('ref_axis',(1.,0.,0.));
#16128=DIRECTION('center_axis',(0.,1.,0.));
#16129=DIRECTION('ref_axis',(1.,0.,0.));
#16130=DIRECTION('center_axis',(0.,-1.,0.));
#16131=DIRECTION('ref_axis',(1.,0.,0.));
#16132=DIRECTION('center_axis',(0.,1.,0.));
#16133=DIRECTION('ref_axis',(1.,0.,0.));
#16134=DIRECTION('center_axis',(0.,-1.,0.));
#16135=DIRECTION('ref_axis',(1.,0.,0.));
#16136=DIRECTION('',(0.,-1.,0.));
#16137=DIRECTION('center_axis',(0.,1.,0.));
#16138=DIRECTION('ref_axis',(1.,0.,0.));
#16139=DIRECTION('axis',(0.,0.,1.));
#16140=DIRECTION('refdir',(1.,0.,0.));
#16141=DIRECTION('center_axis',(0.,0.,1.));
#16142=DIRECTION('ref_axis',(1.,0.,0.));
#16143=DIRECTION('center_axis',(0.,0.,1.));
#16144=DIRECTION('ref_axis',(1.,0.,0.));
#16145=DIRECTION('',(0.,0.,1.));
#16146=DIRECTION('center_axis',(0.,0.,1.));
#16147=DIRECTION('ref_axis',(1.,0.,0.));
#16148=DIRECTION('center_axis',(0.,0.,1.));
#16149=DIRECTION('ref_axis',(1.,0.,0.));
#16150=DIRECTION('center_axis',(0.,0.,1.));
#16151=DIRECTION('ref_axis',(1.,0.,0.));
#16152=DIRECTION('center_axis',(0.,0.,1.));
#16153=DIRECTION('ref_axis',(1.,0.,0.));
#16154=DIRECTION('',(0.,0.,1.));
#16155=DIRECTION('center_axis',(0.,0.,1.));
#16156=DIRECTION('ref_axis',(1.,0.,0.));
#16157=DIRECTION('center_axis',(0.,0.,1.));
#16158=DIRECTION('ref_axis',(1.,0.,0.));
#16159=DIRECTION('center_axis',(1.,0.,0.));
#16160=DIRECTION('ref_axis',(0.,0.,-1.));
#16161=DIRECTION('center_axis',(1.,0.,0.));
#16162=DIRECTION('ref_axis',(0.,0.,-1.));
#16163=DIRECTION('',(1.,0.,0.));
#16164=DIRECTION('center_axis',(-1.,0.,0.));
#16165=DIRECTION('ref_axis',(0.,0.,-1.));
#16166=DIRECTION('center_axis',(0.,1.,0.));
#16167=DIRECTION('ref_axis',(-1.,0.,0.));
#16168=DIRECTION('',(-1.,0.,0.));
#16169=DIRECTION('',(0.,0.,1.));
#16170=DIRECTION('',(-1.,0.,0.));
#16171=DIRECTION('',(0.,0.,1.));
#16172=DIRECTION('center_axis',(1.,0.,0.));
#16173=DIRECTION('ref_axis',(0.,1.,0.));
#16174=DIRECTION('',(0.,1.,0.));
#16175=DIRECTION('',(0.,1.,0.));
#16176=DIRECTION('',(0.,0.,1.));
#16177=DIRECTION('center_axis',(0.,-1.,0.));
#16178=DIRECTION('ref_axis',(1.,0.,0.));
#16179=DIRECTION('',(1.,0.,0.));
#16180=DIRECTION('',(1.,0.,0.));
#16181=DIRECTION('',(0.,0.,1.));
#16182=DIRECTION('center_axis',(-1.,0.,0.));
#16183=DIRECTION('ref_axis',(0.,-1.,0.));
#16184=DIRECTION('',(0.,-1.,0.));
#16185=DIRECTION('',(0.,-1.,0.));
#16186=DIRECTION('center_axis',(0.,0.,1.));
#16187=DIRECTION('ref_axis',(1.,0.,0.));
#16188=DIRECTION('center_axis',(0.,0.,1.));
#16189=DIRECTION('ref_axis',(1.,0.,0.));
#16190=DIRECTION('axis',(0.,0.,1.));
#16191=DIRECTION('refdir',(1.,0.,0.));
#16192=DIRECTION('center_axis',(1.,0.,0.));
#16193=DIRECTION('ref_axis',(0.,0.,-1.));
#16194=DIRECTION('center_axis',(1.,0.,0.));
#16195=DIRECTION('ref_axis',(0.,0.,-1.));
#16196=DIRECTION('center_axis',(1.,0.,0.));
#16197=DIRECTION('ref_axis',(0.,0.,-1.));
#16198=DIRECTION('',(-1.,0.,0.));
#16199=DIRECTION('center_axis',(1.,0.,0.));
#16200=DIRECTION('ref_axis',(0.,0.,-1.));
#16201=DIRECTION('center_axis',(1.,0.,0.));
#16202=DIRECTION('ref_axis',(0.,0.,-1.));
#16203=DIRECTION('axis',(0.,0.,1.));
#16204=DIRECTION('refdir',(1.,0.,0.));
#16205=DIRECTION('center_axis',(0.,0.,1.));
#16206=DIRECTION('ref_axis',(1.,0.,0.));
#16207=DIRECTION('',(1.,0.,0.));
#16208=DIRECTION('center_axis',(0.,0.,1.));
#16209=DIRECTION('ref_axis',(1.,0.,0.));
#16210=DIRECTION('center_axis',(0.,0.,1.));
#16211=DIRECTION('ref_axis',(1.,0.,0.));
#16212=DIRECTION('center_axis',(0.,0.,1.));
#16213=DIRECTION('ref_axis',(1.,0.,0.));
#16214=DIRECTION('',(0.,0.,1.));
#16215=DIRECTION('center_axis',(0.,0.,-1.));
#16216=DIRECTION('ref_axis',(1.,0.,0.));
#16217=DIRECTION('center_axis',(0.,0.,1.));
#16218=DIRECTION('ref_axis',(1.,0.,0.));
#16219=DIRECTION('',(-1.,0.,0.));
#16220=DIRECTION('center_axis',(1.,0.,0.));
#16221=DIRECTION('ref_axis',(0.,0.,-1.));
#16222=DIRECTION('center_axis',(1.,0.,0.));
#16223=DIRECTION('ref_axis',(0.,0.,-1.));
#16224=DIRECTION('',(1.,0.,0.));
#16225=DIRECTION('',(1.,0.,0.));
#16226=DIRECTION('center_axis',(-1.,0.,0.));
#16227=DIRECTION('ref_axis',(0.,0.,-1.));
#16228=DIRECTION('center_axis',(0.,1.,0.));
#16229=DIRECTION('ref_axis',(-1.,0.,0.));
#16230=DIRECTION('',(-1.,0.,0.));
#16231=DIRECTION('',(0.,0.,1.));
#16232=DIRECTION('',(-1.,0.,0.));
#16233=DIRECTION('',(0.,0.,1.));
#16234=DIRECTION('center_axis',(1.,0.,0.));
#16235=DIRECTION('ref_axis',(0.,1.,0.));
#16236=DIRECTION('',(0.,1.,0.));
#16237=DIRECTION('',(0.,1.,0.));
#16238=DIRECTION('',(0.,0.,1.));
#16239=DIRECTION('center_axis',(0.,-1.,0.));
#16240=DIRECTION('ref_axis',(1.,0.,0.));
#16241=DIRECTION('',(1.,0.,0.));
#16242=DIRECTION('',(1.,0.,0.));
#16243=DIRECTION('',(0.,0.,1.));
#16244=DIRECTION('center_axis',(-1.,0.,0.));
#16245=DIRECTION('ref_axis',(0.,-1.,0.));
#16246=DIRECTION('',(0.,-1.,0.));
#16247=DIRECTION('',(0.,-1.,0.));
#16248=DIRECTION('center_axis',(0.,0.,1.));
#16249=DIRECTION('ref_axis',(1.,0.,0.));
#16250=DIRECTION('center_axis',(0.,0.,1.));
#16251=DIRECTION('ref_axis',(1.,0.,0.));
#16252=DIRECTION('axis',(0.,0.,1.));
#16253=DIRECTION('refdir',(1.,0.,0.));
#16254=DIRECTION('axis',(0.,0.,1.));
#16255=DIRECTION('refdir',(1.,0.,0.));
#16256=DIRECTION('center_axis',(0.,0.,1.));
#16257=DIRECTION('ref_axis',(1.,0.,0.));
#16258=DIRECTION('',(-1.,0.,0.));
#16259=DIRECTION('center_axis',(0.,0.,1.));
#16260=DIRECTION('ref_axis',(1.,0.,0.));
#16261=DIRECTION('center_axis',(0.,0.,1.));
#16262=DIRECTION('ref_axis',(1.,0.,0.));
#16263=DIRECTION('',(0.,0.,-1.));
#16264=DIRECTION('center_axis',(0.,0.,1.));
#16265=DIRECTION('ref_axis',(1.,0.,0.));
#16266=DIRECTION('',(0.,0.,1.));
#16267=DIRECTION('center_axis',(0.,0.,-1.));
#16268=DIRECTION('ref_axis',(1.,0.,0.));
#16269=DIRECTION('center_axis',(0.,0.,1.));
#16270=DIRECTION('ref_axis',(1.,0.,0.));
#16271=DIRECTION('',(0.,0.,1.));
#16272=DIRECTION('center_axis',(0.,0.,1.));
#16273=DIRECTION('ref_axis',(1.,0.,0.));
#16274=DIRECTION('',(1.,0.,0.));
#16275=DIRECTION('center_axis',(0.,0.,1.));
#16276=DIRECTION('ref_axis',(1.,0.,0.));
#16277=DIRECTION('center_axis',(0.,0.,1.));
#16278=DIRECTION('ref_axis',(1.,0.,0.));
#16279=DIRECTION('',(0.,0.,-1.));
#16280=DIRECTION('center_axis',(0.,0.,1.));
#16281=DIRECTION('ref_axis',(1.,0.,0.));
#16282=DIRECTION('',(0.,0.,1.));
#16283=DIRECTION('center_axis',(0.,0.,-1.));
#16284=DIRECTION('ref_axis',(1.,0.,0.));
#16285=DIRECTION('center_axis',(0.,0.,1.));
#16286=DIRECTION('ref_axis',(1.,0.,0.));
#16287=DIRECTION('',(0.,0.,1.));
#16288=DIRECTION('center_axis',(0.,0.,1.));
#16289=DIRECTION('ref_axis',(1.,0.,0.));
#16290=DIRECTION('',(-1.,0.,0.));
#16291=DIRECTION('center_axis',(0.,0.,1.));
#16292=DIRECTION('ref_axis',(1.,0.,0.));
#16293=DIRECTION('center_axis',(0.,0.,1.));
#16294=DIRECTION('ref_axis',(1.,0.,0.));
#16295=DIRECTION('',(0.,0.,-1.));
#16296=DIRECTION('center_axis',(0.,0.,1.));
#16297=DIRECTION('ref_axis',(1.,0.,0.));
#16298=DIRECTION('',(0.,0.,1.));
#16299=DIRECTION('center_axis',(0.,0.,-1.));
#16300=DIRECTION('ref_axis',(1.,0.,0.));
#16301=DIRECTION('center_axis',(0.,0.,1.));
#16302=DIRECTION('ref_axis',(1.,0.,0.));
#16303=DIRECTION('',(0.,0.,1.));
#16304=DIRECTION('center_axis',(0.,0.,1.));
#16305=DIRECTION('ref_axis',(1.,0.,0.));
#16306=DIRECTION('',(1.,0.,0.));
#16307=DIRECTION('center_axis',(0.,0.,1.));
#16308=DIRECTION('ref_axis',(1.,0.,0.));
#16309=DIRECTION('center_axis',(0.,0.,1.));
#16310=DIRECTION('ref_axis',(1.,0.,0.));
#16311=DIRECTION('',(0.,0.,-1.));
#16312=DIRECTION('center_axis',(0.,0.,1.));
#16313=DIRECTION('ref_axis',(1.,0.,0.));
#16314=DIRECTION('',(0.,0.,1.));
#16315=DIRECTION('center_axis',(0.,0.,-1.));
#16316=DIRECTION('ref_axis',(1.,0.,0.));
#16317=DIRECTION('center_axis',(0.,0.,1.));
#16318=DIRECTION('ref_axis',(1.,0.,0.));
#16319=DIRECTION('',(0.,0.,1.));
#16320=DIRECTION('center_axis',(0.,-1.,0.));
#16321=DIRECTION('ref_axis',(0.,0.,-1.));
#16322=DIRECTION('',(-1.,0.,0.));
#16323=DIRECTION('',(-1.,0.,0.));
#16324=DIRECTION('',(0.,0.,1.));
#16325=DIRECTION('',(1.,0.,0.));
#16326=DIRECTION('',(0.,0.,-1.));
#16327=DIRECTION('',(-1.,0.,0.));
#16328=DIRECTION('center_axis',(0.,1.,0.));
#16329=DIRECTION('ref_axis',(0.,0.,1.));
#16330=DIRECTION('',(1.,0.,0.));
#16331=DIRECTION('',(1.,0.,0.));
#16332=DIRECTION('',(0.,0.,1.));
#16333=DIRECTION('',(1.,0.,0.));
#16334=DIRECTION('',(0.,0.,-1.));
#16335=DIRECTION('',(1.,0.,0.));
#16336=DIRECTION('center_axis',(-1.,0.,0.));
#16337=DIRECTION('ref_axis',(0.,0.,1.));
#16338=DIRECTION('',(0.,-1.,0.));
#16339=DIRECTION('',(0.,0.,1.));
#16340=DIRECTION('',(0.,1.,0.));
#16341=DIRECTION('',(0.,0.,-1.));
#16342=DIRECTION('',(0.,-1.,0.));
#16343=DIRECTION('',(0.,-1.,0.));
#16344=DIRECTION('',(0.,0.,1.));
#16345=DIRECTION('',(0.,-1.,0.));
#16346=DIRECTION('',(0.,0.,-1.));
#16347=DIRECTION('',(0.,-1.,0.));
#16348=DIRECTION('center_axis',(0.,0.,-1.));
#16349=DIRECTION('ref_axis',(0.,1.,0.));
#16350=DIRECTION('',(0.,1.,0.));
#16351=DIRECTION('',(1.,0.,0.));
#16352=DIRECTION('center_axis',(0.,-1.,0.));
#16353=DIRECTION('ref_axis',(0.,0.,-1.));
#16354=DIRECTION('',(0.,0.,-1.));
#16355=DIRECTION('',(1.,0.,0.));
#16356=DIRECTION('center_axis',(0.,0.,1.));
#16357=DIRECTION('ref_axis',(0.,-1.,0.));
#16358=DIRECTION('',(0.,-1.,0.));
#16359=DIRECTION('',(1.,0.,0.));
#16360=DIRECTION('center_axis',(0.,1.,0.));
#16361=DIRECTION('ref_axis',(0.,0.,1.));
#16362=DIRECTION('',(0.,0.,1.));
#16363=DIRECTION('',(1.,0.,0.));
#16364=DIRECTION('center_axis',(0.,0.,-1.));
#16365=DIRECTION('ref_axis',(0.,1.,0.));
#16366=DIRECTION('',(0.,1.,0.));
#16367=DIRECTION('center_axis',(0.,0.,-1.));
#16368=DIRECTION('ref_axis',(0.,1.,0.));
#16369=DIRECTION('',(0.,1.,0.));
#16370=DIRECTION('',(1.,0.,0.));
#16371=DIRECTION('center_axis',(0.,-1.,0.));
#16372=DIRECTION('ref_axis',(0.,0.,-1.));
#16373=DIRECTION('',(0.,0.,-1.));
#16374=DIRECTION('',(1.,0.,0.));
#16375=DIRECTION('center_axis',(0.,0.,-1.));
#16376=DIRECTION('ref_axis',(0.,1.,0.));
#16377=DIRECTION('',(0.,1.,0.));
#16378=DIRECTION('',(1.,0.,0.));
#16379=DIRECTION('center_axis',(0.,1.,0.));
#16380=DIRECTION('ref_axis',(0.,0.,1.));
#16381=DIRECTION('',(0.,0.,1.));
#16382=DIRECTION('',(1.,0.,0.));
#16383=DIRECTION('center_axis',(0.,0.,-1.));
#16384=DIRECTION('ref_axis',(0.,1.,0.));
#16385=DIRECTION('',(0.,1.,0.));
#16386=DIRECTION('center_axis',(1.,0.,0.));
#16387=DIRECTION('ref_axis',(0.,0.,-1.));
#16388=DIRECTION('axis',(0.,0.,1.));
#16389=DIRECTION('refdir',(1.,0.,0.));
#16390=DIRECTION('center_axis',(0.,0.,1.));
#16391=DIRECTION('ref_axis',(0.,-1.,0.));
#16392=DIRECTION('',(0.,-1.,0.));
#16393=DIRECTION('',(1.,0.,0.));
#16394=DIRECTION('',(0.,-1.,0.));
#16395=DIRECTION('',(1.,0.,0.));
#16396=DIRECTION('center_axis',(0.,1.,0.));
#16397=DIRECTION('ref_axis',(0.,0.,1.));
#16398=DIRECTION('',(0.,0.,1.));
#16399=DIRECTION('',(0.,0.,1.));
#16400=DIRECTION('',(1.,0.,0.));
#16401=DIRECTION('center_axis',(0.,0.,-1.));
#16402=DIRECTION('ref_axis',(0.,1.,0.));
#16403=DIRECTION('',(0.,1.,0.));
#16404=DIRECTION('',(0.,1.,0.));
#16405=DIRECTION('',(1.,0.,0.));
#16406=DIRECTION('center_axis',(0.,-1.,0.));
#16407=DIRECTION('ref_axis',(0.,0.,-1.));
#16408=DIRECTION('',(0.,0.,-1.));
#16409=DIRECTION('',(0.,0.,-1.));
#16410=DIRECTION('',(1.,0.,0.));
#16411=DIRECTION('center_axis',(0.,0.,-1.));
#16412=DIRECTION('ref_axis',(0.,1.,0.));
#16413=DIRECTION('',(0.,1.,0.));
#16414=DIRECTION('',(0.,1.,0.));
#16415=DIRECTION('',(1.,0.,0.));
#16416=DIRECTION('center_axis',(0.,1.,0.));
#16417=DIRECTION('ref_axis',(0.,0.,1.));
#16418=DIRECTION('',(0.,0.,1.));
#16419=DIRECTION('',(0.,0.,1.));
#16420=DIRECTION('',(1.,0.,0.));
#16421=DIRECTION('center_axis',(0.,0.,-1.));
#16422=DIRECTION('ref_axis',(0.,1.,0.));
#16423=DIRECTION('',(0.,1.,0.));
#16424=DIRECTION('',(0.,1.,0.));
#16425=DIRECTION('',(1.,0.,0.));
#16426=DIRECTION('center_axis',(0.,-1.,0.));
#16427=DIRECTION('ref_axis',(0.,0.,-1.));
#16428=DIRECTION('',(0.,0.,-1.));
#16429=DIRECTION('',(0.,0.,-1.));
#16430=DIRECTION('center_axis',(1.,0.,0.));
#16431=DIRECTION('ref_axis',(0.,0.,-1.));
#16432=DIRECTION('center_axis',(1.,0.,0.));
#16433=DIRECTION('ref_axis',(0.,0.,-1.));
#16434=DIRECTION('axis',(0.,0.,1.));
#16435=DIRECTION('refdir',(1.,0.,0.));
#16436=DIRECTION('center_axis',(0.,0.,-1.));
#16437=DIRECTION('ref_axis',(0.,-1.,0.));
#16438=DIRECTION('',(0.,1.,0.));
#16439=DIRECTION('',(-1.,0.,0.));
#16440=DIRECTION('',(0.,-1.,0.));
#16441=DIRECTION('',(-1.,0.,0.));
#16442=DIRECTION('center_axis',(0.,1.,0.));
#16443=DIRECTION('ref_axis',(0.,0.,-1.));
#16444=DIRECTION('',(0.,0.,1.));
#16445=DIRECTION('',(0.,0.,-1.));
#16446=DIRECTION('',(-1.,0.,0.));
#16447=DIRECTION('center_axis',(0.,0.,-1.));
#16448=DIRECTION('ref_axis',(0.,-1.,0.));
#16449=DIRECTION('',(0.,1.,0.));
#16450=DIRECTION('',(0.,-1.,0.));
#16451=DIRECTION('',(-1.,0.,0.));
#16452=DIRECTION('center_axis',(0.,-1.,0.));
#16453=DIRECTION('ref_axis',(0.,0.,1.));
#16454=DIRECTION('',(0.,0.,-1.));
#16455=DIRECTION('',(0.,0.,1.));
#16456=DIRECTION('',(-1.,0.,0.));
#16457=DIRECTION('center_axis',(0.,0.,-1.));
#16458=DIRECTION('ref_axis',(0.,-1.,0.));
#16459=DIRECTION('',(0.,1.,0.));
#16460=DIRECTION('',(0.,-1.,0.));
#16461=DIRECTION('',(-1.,0.,0.));
#16462=DIRECTION('center_axis',(0.,1.,0.));
#16463=DIRECTION('ref_axis',(0.,0.,-1.));
#16464=DIRECTION('',(0.,0.,1.));
#16465=DIRECTION('',(0.,0.,-1.));
#16466=DIRECTION('',(-1.,0.,0.));
#16467=DIRECTION('center_axis',(0.,0.,1.));
#16468=DIRECTION('ref_axis',(0.,1.,0.));
#16469=DIRECTION('',(0.,-1.,0.));
#16470=DIRECTION('',(0.,1.,0.));
#16471=DIRECTION('',(-1.,0.,0.));
#16472=DIRECTION('center_axis',(0.,-1.,0.));
#16473=DIRECTION('ref_axis',(0.,0.,1.));
#16474=DIRECTION('',(0.,0.,-1.));
#16475=DIRECTION('',(0.,0.,1.));
#16476=DIRECTION('center_axis',(1.,0.,0.));
#16477=DIRECTION('ref_axis',(0.,0.,-1.));
#16478=DIRECTION('center_axis',(-1.,0.,0.));
#16479=DIRECTION('ref_axis',(0.,0.,1.));
#16480=DIRECTION('',(0.,0.,1.));
#16481=DIRECTION('',(1.,0.,0.));
#16482=DIRECTION('',(0.,0.,1.));
#16483=DIRECTION('',(1.,0.,0.));
#16484=DIRECTION('',(0.,0.,1.));
#16485=DIRECTION('',(1.,0.,0.));
#16486=DIRECTION('axis',(0.,0.,1.));
#16487=DIRECTION('refdir',(1.,0.,0.));
#16488=DIRECTION('center_axis',(0.866025403784439,0.,-0.5));
#16489=DIRECTION('ref_axis',(0.5,0.,0.866025403784439));
#16490=DIRECTION('',(-0.5,0.,-0.866025403784439));
#16491=DIRECTION('',(0.,-1.,0.));
#16492=DIRECTION('',(0.5,0.,0.866025403784439));
#16493=DIRECTION('',(0.,-1.,0.));
#16494=DIRECTION('center_axis',(1.20185167898973E-16,0.,-1.));
#16495=DIRECTION('ref_axis',(1.,0.,1.20185167898973E-16));
#16496=DIRECTION('',(-1.,0.,-1.20185167898973E-16));
#16497=DIRECTION('',(0.,-1.,0.));
#16498=DIRECTION('',(1.,0.,1.20185167898973E-16));
#16499=DIRECTION('center_axis',(-0.866025403784439,0.,-0.5));
#16500=DIRECTION('ref_axis',(0.5,0.,-0.866025403784439));
#16501=DIRECTION('',(-0.5,0.,0.866025403784439));
#16502=DIRECTION('',(0.,-1.,0.));
#16503=DIRECTION('',(0.5,0.,-0.866025403784439));
#16504=DIRECTION('center_axis',(-0.866025403784439,0.,0.5));
#16505=DIRECTION('ref_axis',(-0.5,0.,-0.866025403784439));
#16506=DIRECTION('',(0.5,0.,0.866025403784439));
#16507=DIRECTION('',(0.,-1.,0.));
#16508=DIRECTION('',(-0.5,0.,-0.866025403784439));
#16509=DIRECTION('center_axis',(-2.40370335797945E-16,0.,1.));
#16510=DIRECTION('ref_axis',(-1.,0.,-2.40370335797945E-16));
#16511=DIRECTION('',(1.,0.,2.40370335797945E-16));
#16512=DIRECTION('',(0.,-1.,0.));
#16513=DIRECTION('',(-1.,0.,-2.40370335797945E-16));
#16514=DIRECTION('center_axis',(0.866025403784439,0.,0.5));
#16515=DIRECTION('ref_axis',(-0.5,0.,0.866025403784439));
#16516=DIRECTION('',(0.5,0.,-0.866025403784439));
#16517=DIRECTION('',(-0.5,0.,0.866025403784439));
#16518=DIRECTION('center_axis',(0.,1.,0.));
#16519=DIRECTION('ref_axis',(1.,0.,0.));
#16520=DIRECTION('center_axis',(0.,-1.,0.));
#16521=DIRECTION('ref_axis',(0.,0.,-1.));
#16522=DIRECTION('center_axis',(0.,1.,0.));
#16523=DIRECTION('ref_axis',(1.,0.,0.));
#16524=DIRECTION('center_axis',(0.,1.,0.));
#16525=DIRECTION('ref_axis',(1.,0.,0.));
#16526=DIRECTION('center_axis',(0.,1.,0.));
#16527=DIRECTION('ref_axis',(0.,0.,1.));
#16528=DIRECTION('center_axis',(0.,-1.,0.));
#16529=DIRECTION('ref_axis',(1.,0.,0.));
#16530=DIRECTION('center_axis',(0.,-1.,0.));
#16531=DIRECTION('ref_axis',(1.,0.,0.));
#16532=DIRECTION('center_axis',(0.,-1.,0.));
#16533=DIRECTION('ref_axis',(1.,0.,0.));
#16534=DIRECTION('',(0.707106781186548,0.707106781186547,8.65956056235493E-17));
#16535=DIRECTION('center_axis',(0.,-1.,0.));
#16536=DIRECTION('ref_axis',(1.,0.,0.));
#16537=DIRECTION('center_axis',(0.,-1.,0.));
#16538=DIRECTION('ref_axis',(1.,0.,0.));
#16539=DIRECTION('',(0.,1.,0.));
#16540=DIRECTION('center_axis',(0.,1.,0.));
#16541=DIRECTION('ref_axis',(1.,0.,0.));
#16542=DIRECTION('center_axis',(0.,-1.,0.));
#16543=DIRECTION('ref_axis',(1.,0.,0.));
#16544=DIRECTION('',(-0.707106781186547,0.707106781186548,-8.65956056235493E-17));
#16545=DIRECTION('center_axis',(0.,-1.,0.));
#16546=DIRECTION('ref_axis',(0.,0.,-1.));
#16547=DIRECTION('center_axis',(0.,-1.,0.));
#16548=DIRECTION('ref_axis',(1.,0.,0.));
#16549=DIRECTION('center_axis',(0.,1.,0.));
#16550=DIRECTION('ref_axis',(1.,0.,0.));
#16551=DIRECTION('center_axis',(0.,1.,0.));
#16552=DIRECTION('ref_axis',(1.,0.,0.));
#16553=DIRECTION('',(-0.447213595499958,0.894427190999916,-5.47678698264203E-17));
#16554=DIRECTION('center_axis',(0.,-1.,0.));
#16555=DIRECTION('ref_axis',(1.,0.,0.));
#16556=DIRECTION('',(0.,1.,0.));
#16557=DIRECTION('axis',(0.,0.,1.));
#16558=DIRECTION('refdir',(1.,0.,0.));
#16559=DIRECTION('axis',(0.,0.,1.));
#16560=DIRECTION('refdir',(1.,0.,0.));
#16561=DIRECTION('center_axis',(0.,-1.,0.));
#16562=DIRECTION('ref_axis',(0.,0.,-1.));
#16563=DIRECTION('center_axis',(0.,-1.,0.));
#16564=DIRECTION('ref_axis',(1.,0.,0.));
#16565=DIRECTION('center_axis',(0.,-1.,0.));
#16566=DIRECTION('ref_axis',(1.,0.,0.));
#16567=DIRECTION('center_axis',(1.,0.,1.22464679914735E-16));
#16568=DIRECTION('ref_axis',(-1.22464679914735E-16,0.,1.));
#16569=DIRECTION('center_axis',(0.,1.,0.));
#16570=DIRECTION('ref_axis',(1.,0.,0.));
#16571=DIRECTION('center_axis',(0.,1.,0.));
#16572=DIRECTION('ref_axis',(1.,0.,0.));
#16573=DIRECTION('center_axis',(0.,-1.,0.));
#16574=DIRECTION('ref_axis',(1.,0.,0.));
#16575=DIRECTION('',(0.,1.,0.));
#16576=DIRECTION('center_axis',(0.,-1.,0.));
#16577=DIRECTION('ref_axis',(1.,0.,0.));
#16578=DIRECTION('center_axis',(0.,-1.,0.));
#16579=DIRECTION('ref_axis',(1.,0.,0.));
#16580=DIRECTION('center_axis',(0.,-1.,0.));
#16581=DIRECTION('ref_axis',(1.,0.,0.));
#16582=DIRECTION('',(0.,1.,0.));
#16583=DIRECTION('center_axis',(0.,-1.,0.));
#16584=DIRECTION('ref_axis',(1.,0.,0.));
#16585=DIRECTION('center_axis',(0.,1.,0.));
#16586=DIRECTION('ref_axis',(1.,0.,0.));
#16587=DIRECTION('',(-0.707106781186548,0.707106781186547,-8.65956056235493E-17));
#16588=DIRECTION('center_axis',(0.,-1.,0.));
#16589=DIRECTION('ref_axis',(1.,0.,0.));
#16590=DIRECTION('center_axis',(0.,1.,0.));
#16591=DIRECTION('ref_axis',(0.,0.,1.));
#16592=DIRECTION('center_axis',(0.,-1.,0.));
#16593=DIRECTION('ref_axis',(1.,0.,0.));
#16594=DIRECTION('center_axis',(0.,-1.,0.));
#16595=DIRECTION('ref_axis',(1.,0.,0.));
#16596=DIRECTION('',(0.,1.,0.));
#16597=DIRECTION('center_axis',(0.,-1.,0.));
#16598=DIRECTION('ref_axis',(0.,0.,-1.));
#16599=DIRECTION('center_axis',(0.,-1.,0.));
#16600=DIRECTION('ref_axis',(1.,0.,0.));
#16601=DIRECTION('center_axis',(0.,-1.,0.));
#16602=DIRECTION('ref_axis',(1.,0.,0.));
#16603=DIRECTION('',(0.707106781186548,0.707106781186547,8.65956056235493E-17));
#16604=DIRECTION('axis',(0.,0.,1.));
#16605=DIRECTION('refdir',(1.,0.,0.));
#16606=DIRECTION('center_axis',(0.,-1.,0.));
#16607=DIRECTION('ref_axis',(0.,0.,-1.));
#16608=DIRECTION('center_axis',(0.,-1.,0.));
#16609=DIRECTION('ref_axis',(1.,0.,0.));
#16610=DIRECTION('center_axis',(0.,-1.,0.));
#16611=DIRECTION('ref_axis',(1.,0.,0.));
#16612=DIRECTION('center_axis',(1.,0.,1.22464679914735E-16));
#16613=DIRECTION('ref_axis',(-1.22464679914735E-16,0.,1.));
#16614=DIRECTION('center_axis',(0.,1.,0.));
#16615=DIRECTION('ref_axis',(1.,0.,0.));
#16616=DIRECTION('center_axis',(0.,1.,0.));
#16617=DIRECTION('ref_axis',(1.,0.,0.));
#16618=DIRECTION('center_axis',(0.,-1.,0.));
#16619=DIRECTION('ref_axis',(1.,0.,0.));
#16620=DIRECTION('center_axis',(0.,-1.,0.));
#16621=DIRECTION('ref_axis',(1.,0.,0.));
#16622=DIRECTION('',(0.,1.,0.));
#16623=DIRECTION('center_axis',(0.,1.,0.));
#16624=DIRECTION('ref_axis',(0.,0.,1.));
#16625=DIRECTION('center_axis',(0.,-1.,0.));
#16626=DIRECTION('ref_axis',(1.,0.,0.));
#16627=DIRECTION('center_axis',(0.,-1.,0.));
#16628=DIRECTION('ref_axis',(1.,0.,0.));
#16629=DIRECTION('center_axis',(0.,-1.,0.));
#16630=DIRECTION('ref_axis',(1.,0.,0.));
#16631=DIRECTION('center_axis',(0.,-1.,0.));
#16632=DIRECTION('ref_axis',(1.,0.,0.));
#16633=DIRECTION('',(0.707106781186548,0.707106781186547,8.65956056235494E-17));
#16634=DIRECTION('center_axis',(0.,-1.,0.));
#16635=DIRECTION('ref_axis',(1.,0.,0.));
#16636=DIRECTION('center_axis',(0.,-1.,0.));
#16637=DIRECTION('ref_axis',(1.,0.,0.));
#16638=DIRECTION('',(0.,1.,0.));
#16639=DIRECTION('center_axis',(0.,1.,0.));
#16640=DIRECTION('ref_axis',(1.,0.,0.));
#16641=DIRECTION('center_axis',(0.,-1.,0.));
#16642=DIRECTION('ref_axis',(1.,0.,0.));
#16643=DIRECTION('',(-0.707106781186548,0.707106781186547,-8.65956056235494E-17));
#16644=DIRECTION('center_axis',(0.,-1.,0.));
#16645=DIRECTION('ref_axis',(0.,0.,-1.));
#16646=DIRECTION('center_axis',(0.,-1.,0.));
#16647=DIRECTION('ref_axis',(1.,0.,0.));
#16648=DIRECTION('',(0.,1.,0.));
#16649=DIRECTION('axis',(0.,0.,1.));
#16650=DIRECTION('refdir',(1.,0.,0.));
#16651=DIRECTION('center_axis',(0.,0.,1.));
#16652=DIRECTION('ref_axis',(1.,0.,0.));
#16653=DIRECTION('center_axis',(1.22464679914735E-16,-1.,0.));
#16654=DIRECTION('ref_axis',(-1.,-1.22464679914735E-16,0.));
#16655=DIRECTION('center_axis',(0.78183148246803,0.,0.623489801858733));
#16656=DIRECTION('ref_axis',(0.623489801858734,0.,-0.78183148246803));
#16657=DIRECTION('center_axis',(7.63554790147315E-17,-1.,-9.57467422477103E-17));
#16658=DIRECTION('ref_axis',(-0.623489801858734,-1.22464679914735E-16,0.78183148246803));
#16659=DIRECTION('center_axis',(0.974927912181824,0.,-0.222520933956314));
#16660=DIRECTION('ref_axis',(-0.222520933956314,0.,-0.974927912181824));
#16661=DIRECTION('center_axis',(-2.7250954951288E-17,-1.,-1.19394234705288E-16));
#16662=DIRECTION('ref_axis',(0.222520933956314,-1.22464679914735E-16,0.974927912181824));
#16663=DIRECTION('center_axis',(0.433883739117558,0.,-0.900968867902419));
#16664=DIRECTION('ref_axis',(-0.900968867902419,0.,-0.433883739117558));
#16665=DIRECTION('center_axis',(-1.10336864020811E-16,-1.,-5.31354332312403E-17));
#16666=DIRECTION('ref_axis',(0.900968867902419,-1.22464679914735E-16,0.433883739117558));
#16667=DIRECTION('center_axis',(-0.433883739117558,0.,-0.900968867902419));
#16668=DIRECTION('ref_axis',(-0.900968867902419,0.,0.433883739117558));
#16669=DIRECTION('center_axis',(-1.10336864020811E-16,-1.,5.31354332312403E-17));
#16670=DIRECTION('ref_axis',(0.900968867902419,-1.22464679914735E-16,-0.433883739117558));
#16671=DIRECTION('center_axis',(-0.974927912181824,0.,-0.222520933956314));
#16672=DIRECTION('ref_axis',(-0.222520933956315,0.,0.974927912181824));
#16673=DIRECTION('center_axis',(-2.7250954951288E-17,-1.,1.19394234705288E-16));
#16674=DIRECTION('ref_axis',(0.222520933956315,-1.22464679914735E-16,-0.974927912181824));
#16675=DIRECTION('center_axis',(-0.78183148246803,0.,0.623489801858734));
#16676=DIRECTION('ref_axis',(0.623489801858733,0.,0.78183148246803));
#16677=DIRECTION('center_axis',(7.63554790147315E-17,-1.,9.57467422477103E-17));
#16678=DIRECTION('ref_axis',(-0.623489801858733,-1.22464679914735E-16,-0.78183148246803));
#16679=DIRECTION('axis',(0.,0.,1.));
#16680=DIRECTION('refdir',(1.,0.,0.));
#16681=DIRECTION('center_axis',(0.,0.,1.));
#16682=DIRECTION('ref_axis',(1.,0.,0.));
#16683=DIRECTION('center_axis',(0.,-1.,0.));
#16684=DIRECTION('ref_axis',(0.,0.,-1.));
#16685=DIRECTION('center_axis',(0.,-1.,0.));
#16686=DIRECTION('ref_axis',(0.,0.,-1.));
#16687=DIRECTION('center_axis',(0.,1.,0.));
#16688=DIRECTION('ref_axis',(1.,0.,0.));
#16689=DIRECTION('center_axis',(0.,1.,0.));
#16690=DIRECTION('ref_axis',(1.,0.,0.));
#16691=DIRECTION('center_axis',(0.,1.,0.));
#16692=DIRECTION('ref_axis',(1.,0.,0.));
#16693=DIRECTION('center_axis',(0.,1.,0.));
#16694=DIRECTION('ref_axis',(1.,0.,0.));
#16695=DIRECTION('',(0.,-1.,0.));
#16696=DIRECTION('center_axis',(0.,-1.,0.));
#16697=DIRECTION('ref_axis',(1.,0.,0.));
#16698=DIRECTION('center_axis',(0.,1.,0.));
#16699=DIRECTION('ref_axis',(1.,0.,0.));
#16700=DIRECTION('center_axis',(0.,1.,0.));
#16701=DIRECTION('ref_axis',(1.,0.,0.));
#16702=DIRECTION('center_axis',(0.,1.,0.));
#16703=DIRECTION('ref_axis',(1.,0.,0.));
#16704=DIRECTION('center_axis',(0.,1.,0.));
#16705=DIRECTION('ref_axis',(1.,0.,0.));
#16706=DIRECTION('center_axis',(0.,1.,0.));
#16707=DIRECTION('ref_axis',(1.,0.,0.));
#16708=DIRECTION('center_axis',(0.,1.,0.));
#16709=DIRECTION('ref_axis',(1.,0.,0.));
#16710=DIRECTION('center_axis',(0.,-1.,0.));
#16711=DIRECTION('ref_axis',(1.,0.,0.));
#16712=DIRECTION('center_axis',(0.,-1.,0.));
#16713=DIRECTION('ref_axis',(0.,0.,-1.));
#16714=DIRECTION('center_axis',(8.96625347776458E-17,0.,1.));
#16715=DIRECTION('ref_axis',(1.,0.,0.));
#16716=DIRECTION('center_axis',(0.,-1.,0.));
#16717=DIRECTION('ref_axis',(0.,0.,-1.));
#16718=DIRECTION('center_axis',(0.,1.,0.));
#16719=DIRECTION('ref_axis',(1.,0.,0.));
#16720=DIRECTION('center_axis',(0.,-1.,0.));
#16721=DIRECTION('ref_axis',(1.,0.,0.));
#16722=DIRECTION('center_axis',(0.,-1.,0.));
#16723=DIRECTION('ref_axis',(0.,0.,-1.));
#16724=DIRECTION('center_axis',(0.,0.,1.));
#16725=DIRECTION('ref_axis',(1.,0.,0.));
#16726=DIRECTION('center_axis',(0.,-1.,0.));
#16727=DIRECTION('ref_axis',(0.,0.,-1.));
#16728=DIRECTION('center_axis',(0.,1.,0.));
#16729=DIRECTION('ref_axis',(1.,0.,0.));
#16730=DIRECTION('center_axis',(0.,-1.,0.));
#16731=DIRECTION('ref_axis',(1.,0.,0.));
#16732=DIRECTION('center_axis',(0.,-1.,0.));
#16733=DIRECTION('ref_axis',(1.,0.,0.));
#16734=DIRECTION('center_axis',(0.,-1.,0.));
#16735=DIRECTION('ref_axis',(0.,0.,-1.));
#16736=DIRECTION('center_axis',(0.,0.,1.));
#16737=DIRECTION('ref_axis',(1.,0.,0.));
#16738=DIRECTION('center_axis',(0.,-1.,0.));
#16739=DIRECTION('ref_axis',(0.,0.,-1.));
#16740=DIRECTION('center_axis',(0.,1.,0.));
#16741=DIRECTION('ref_axis',(1.,0.,0.));
#16742=DIRECTION('center_axis',(0.,-1.,0.));
#16743=DIRECTION('ref_axis',(1.,0.,0.));
#16744=DIRECTION('center_axis',(0.,-1.,0.));
#16745=DIRECTION('ref_axis',(0.,0.,-1.));
#16746=DIRECTION('center_axis',(8.96625347776458E-17,0.,1.));
#16747=DIRECTION('ref_axis',(1.,0.,0.));
#16748=DIRECTION('center_axis',(0.,-1.,0.));
#16749=DIRECTION('ref_axis',(0.,0.,-1.));
#16750=DIRECTION('center_axis',(0.,1.,0.));
#16751=DIRECTION('ref_axis',(1.,0.,0.));
#16752=DIRECTION('center_axis',(0.,-1.,0.));
#16753=DIRECTION('ref_axis',(1.,0.,0.));
#16754=DIRECTION('center_axis',(0.,-1.,0.));
#16755=DIRECTION('ref_axis',(0.,0.,-1.));
#16756=DIRECTION('center_axis',(0.,0.,1.));
#16757=DIRECTION('ref_axis',(1.,0.,0.));
#16758=DIRECTION('center_axis',(0.,-1.,0.));
#16759=DIRECTION('ref_axis',(0.,0.,-1.));
#16760=DIRECTION('center_axis',(0.,1.,0.));
#16761=DIRECTION('ref_axis',(1.,0.,0.));
#16762=DIRECTION('center_axis',(0.,1.,0.));
#16763=DIRECTION('ref_axis',(1.,0.,0.));
#16764=DIRECTION('',(0.,1.,0.));
#16765=DIRECTION('center_axis',(0.,-1.,0.));
#16766=DIRECTION('ref_axis',(1.,0.,0.));
#16767=DIRECTION('center_axis',(0.,-1.,0.));
#16768=DIRECTION('ref_axis',(1.,0.,0.));
#16769=DIRECTION('center_axis',(0.,1.,0.));
#16770=DIRECTION('ref_axis',(1.,0.,0.));
#16771=DIRECTION('center_axis',(0.,-1.,0.));
#16772=DIRECTION('ref_axis',(0.,0.,-1.));
#16773=DIRECTION('center_axis',(0.,0.,1.));
#16774=DIRECTION('ref_axis',(1.,0.,0.));
#16775=DIRECTION('center_axis',(0.,-1.,0.));
#16776=DIRECTION('ref_axis',(0.,0.,-1.));
#16777=DIRECTION('center_axis',(0.,-1.,0.));
#16778=DIRECTION('ref_axis',(-1.,0.,0.));
#16779=DIRECTION('center_axis',(0.,1.,0.));
#16780=DIRECTION('ref_axis',(1.,0.,0.));
#16781=DIRECTION('axis',(0.,0.,1.));
#16782=DIRECTION('refdir',(1.,0.,0.));
#16783=DIRECTION('center_axis',(0.,1.,0.));
#16784=DIRECTION('ref_axis',(0.,0.,1.));
#16785=DIRECTION('center_axis',(0.,-1.,0.));
#16786=DIRECTION('ref_axis',(1.,0.,0.));
#16787=DIRECTION('center_axis',(0.,-1.,0.));
#16788=DIRECTION('ref_axis',(1.,0.,0.));
#16789=DIRECTION('center_axis',(0.,-1.,0.));
#16790=DIRECTION('ref_axis',(1.,0.,0.));
#16791=DIRECTION('center_axis',(0.,-1.,0.));
#16792=DIRECTION('ref_axis',(1.,0.,0.));
#16793=DIRECTION('',(0.,1.,0.));
#16794=DIRECTION('center_axis',(0.,-1.,0.));
#16795=DIRECTION('ref_axis',(0.,0.,-1.));
#16796=DIRECTION('center_axis',(0.,-1.,0.));
#16797=DIRECTION('ref_axis',(1.,0.,0.));
#16798=DIRECTION('center_axis',(0.,-1.,0.));
#16799=DIRECTION('ref_axis',(1.,0.,0.));
#16800=DIRECTION('',(0.,1.,0.));
#16801=DIRECTION('center_axis',(0.,1.,0.));
#16802=DIRECTION('ref_axis',(0.,0.,1.));
#16803=DIRECTION('center_axis',(0.,-1.,0.));
#16804=DIRECTION('ref_axis',(1.,0.,0.));
#16805=DIRECTION('center_axis',(0.,-1.,0.));
#16806=DIRECTION('ref_axis',(1.,0.,0.));
#16807=DIRECTION('center_axis',(0.,-1.,0.));
#16808=DIRECTION('ref_axis',(1.,0.,0.));
#16809=DIRECTION('center_axis',(0.,-1.,0.));
#16810=DIRECTION('ref_axis',(1.,0.,0.));
#16811=DIRECTION('',(0.,1.,0.));
#16812=DIRECTION('center_axis',(0.,-1.,0.));
#16813=DIRECTION('ref_axis',(0.,0.,-1.));
#16814=DIRECTION('center_axis',(0.,-1.,0.));
#16815=DIRECTION('ref_axis',(1.,0.,0.));
#16816=DIRECTION('center_axis',(0.,-1.,0.));
#16817=DIRECTION('ref_axis',(1.,0.,0.));
#16818=DIRECTION('',(0.,1.,0.));
#16819=DIRECTION('',(0.,0.,1.));
#16820=DIRECTION('',(1.,0.,0.));
#16821=DIRECTION('',(0.,0.,1.));
#16822=DIRECTION('',(1.,0.,0.));
#16823=DIRECTION('',(0.,0.,1.));
#16824=DIRECTION('',(1.,0.,0.));
#16825=DIRECTION('',(0.,0.,1.));
#16826=DIRECTION('',(1.,0.,0.));
#16827=DIRECTION('',(0.,0.,1.));
#16828=DIRECTION('',(1.,0.,0.));
#16829=DIRECTION('axis',(0.,0.,1.));
#16830=DIRECTION('refdir',(1.,0.,0.));
#16831=DIRECTION('center_axis',(0.866025403784439,0.,-0.5));
#16832=DIRECTION('ref_axis',(0.5,0.,0.866025403784439));
#16833=DIRECTION('',(-0.5,0.,-0.866025403784439));
#16834=DIRECTION('',(0.,-1.,0.));
#16835=DIRECTION('',(0.5,0.,0.866025403784439));
#16836=DIRECTION('',(0.,-1.,0.));
#16837=DIRECTION('center_axis',(1.60246890531964E-16,0.,-1.));
#16838=DIRECTION('ref_axis',(1.,0.,1.60246890531964E-16));
#16839=DIRECTION('',(-1.,0.,-1.60246890531964E-16));
#16840=DIRECTION('',(0.,-1.,0.));
#16841=DIRECTION('',(1.,0.,1.60246890531964E-16));
#16842=DIRECTION('center_axis',(-0.866025403784439,0.,-0.5));
#16843=DIRECTION('ref_axis',(0.5,0.,-0.866025403784439));
#16844=DIRECTION('',(-0.5,0.,0.866025403784439));
#16845=DIRECTION('',(0.,-1.,0.));
#16846=DIRECTION('',(0.5,0.,-0.866025403784439));
#16847=DIRECTION('center_axis',(-0.866025403784439,0.,0.5));
#16848=DIRECTION('ref_axis',(-0.5,0.,-0.866025403784439));
#16849=DIRECTION('',(0.5,0.,0.866025403784439));
#16850=DIRECTION('',(0.,-1.,0.));
#16851=DIRECTION('',(-0.5,0.,-0.866025403784439));
#16852=DIRECTION('center_axis',(-1.60246890531964E-16,0.,1.));
#16853=DIRECTION('ref_axis',(-1.,0.,-1.60246890531964E-16));
#16854=DIRECTION('',(1.,0.,1.60246890531964E-16));
#16855=DIRECTION('',(0.,-1.,0.));
#16856=DIRECTION('',(-1.,0.,-1.60246890531964E-16));
#16857=DIRECTION('center_axis',(0.866025403784439,0.,0.5));
#16858=DIRECTION('ref_axis',(-0.5,0.,0.866025403784439));
#16859=DIRECTION('',(0.5,0.,-0.866025403784439));
#16860=DIRECTION('',(-0.5,0.,0.866025403784439));
#16861=DIRECTION('center_axis',(0.,1.,0.));
#16862=DIRECTION('ref_axis',(1.,0.,0.));
#16863=DIRECTION('center_axis',(0.,-1.,0.));
#16864=DIRECTION('ref_axis',(0.,0.,-1.));
#16865=DIRECTION('center_axis',(0.,1.,0.));
#16866=DIRECTION('ref_axis',(1.,0.,0.));
#16867=DIRECTION('center_axis',(0.,1.,0.));
#16868=DIRECTION('ref_axis',(1.,0.,0.));
#16869=DIRECTION('center_axis',(0.,1.,0.));
#16870=DIRECTION('ref_axis',(0.,0.,1.));
#16871=DIRECTION('center_axis',(0.,-1.,0.));
#16872=DIRECTION('ref_axis',(1.,0.,0.));
#16873=DIRECTION('center_axis',(0.,-1.,0.));
#16874=DIRECTION('ref_axis',(1.,0.,0.));
#16875=DIRECTION('center_axis',(0.,-1.,0.));
#16876=DIRECTION('ref_axis',(1.,0.,0.));
#16877=DIRECTION('',(0.707106781186547,0.707106781186548,8.65956056235493E-17));
#16878=DIRECTION('center_axis',(0.,-1.,0.));
#16879=DIRECTION('ref_axis',(1.,0.,0.));
#16880=DIRECTION('center_axis',(0.,-1.,0.));
#16881=DIRECTION('ref_axis',(1.,0.,0.));
#16882=DIRECTION('',(0.,1.,0.));
#16883=DIRECTION('center_axis',(0.,1.,0.));
#16884=DIRECTION('ref_axis',(1.,0.,0.));
#16885=DIRECTION('center_axis',(0.,-1.,0.));
#16886=DIRECTION('ref_axis',(1.,0.,0.));
#16887=DIRECTION('',(-0.707106781186547,0.707106781186548,-8.65956056235493E-17));
#16888=DIRECTION('center_axis',(0.,-1.,0.));
#16889=DIRECTION('ref_axis',(0.,0.,-1.));
#16890=DIRECTION('center_axis',(0.,-1.,0.));
#16891=DIRECTION('ref_axis',(1.,0.,0.));
#16892=DIRECTION('center_axis',(0.,1.,0.));
#16893=DIRECTION('ref_axis',(1.,0.,0.));
#16894=DIRECTION('center_axis',(0.,1.,0.));
#16895=DIRECTION('ref_axis',(1.,0.,0.));
#16896=DIRECTION('',(-0.447213595499958,0.894427190999916,-5.47678698264203E-17));
#16897=DIRECTION('center_axis',(0.,-1.,0.));
#16898=DIRECTION('ref_axis',(1.,0.,0.));
#16899=DIRECTION('',(0.,1.,0.));
#16900=DIRECTION('axis',(0.,0.,1.));
#16901=DIRECTION('refdir',(1.,0.,0.));
#16902=DIRECTION('axis',(0.,0.,1.));
#16903=DIRECTION('refdir',(1.,0.,0.));
#16904=DIRECTION('center_axis',(0.,1.,0.));
#16905=DIRECTION('ref_axis',(1.,0.,0.));
#16906=DIRECTION('center_axis',(0.,1.,0.));
#16907=DIRECTION('ref_axis',(1.,0.,0.));
#16908=DIRECTION('',(0.,1.,0.));
#16909=DIRECTION('center_axis',(0.,1.,0.));
#16910=DIRECTION('ref_axis',(1.,0.,0.));
#16911=DIRECTION('center_axis',(0.,1.,0.));
#16912=DIRECTION('ref_axis',(1.,0.,0.));
#16913=DIRECTION('center_axis',(0.,1.,0.));
#16914=DIRECTION('ref_axis',(1.,0.,0.));
#16915=DIRECTION('center_axis',(0.,1.,0.));
#16916=DIRECTION('ref_axis',(1.,0.,0.));
#16917=DIRECTION('center_axis',(0.,1.,0.));
#16918=DIRECTION('ref_axis',(1.,0.,0.));
#16919=DIRECTION('center_axis',(0.,1.,0.));
#16920=DIRECTION('ref_axis',(1.,0.,0.));
#16921=DIRECTION('center_axis',(0.,1.,0.));
#16922=DIRECTION('ref_axis',(1.,0.,0.));
#16923=DIRECTION('center_axis',(0.,-1.,0.));
#16924=DIRECTION('ref_axis',(1.,0.,0.));
#16925=DIRECTION('center_axis',(0.,1.,0.));
#16926=DIRECTION('ref_axis',(1.,0.,0.));
#16927=DIRECTION('',(0.,-1.,0.));
#16928=DIRECTION('center_axis',(0.,1.,0.));
#16929=DIRECTION('ref_axis',(1.,0.,0.));
#16930=DIRECTION('',(0.,-1.,0.));
#16931=DIRECTION('center_axis',(0.,1.,0.));
#16932=DIRECTION('ref_axis',(1.,0.,0.));
#16933=DIRECTION('center_axis',(0.,1.,0.));
#16934=DIRECTION('ref_axis',(1.,0.,0.));
#16935=DIRECTION('center_axis',(0.,1.,0.));
#16936=DIRECTION('ref_axis',(1.,0.,0.));
#16937=DIRECTION('',(0.,-1.,0.));
#16938=DIRECTION('center_axis',(0.,1.,0.));
#16939=DIRECTION('ref_axis',(1.,0.,0.));
#16940=DIRECTION('center_axis',(0.,1.,0.));
#16941=DIRECTION('ref_axis',(1.,0.,0.));
#16942=DIRECTION('center_axis',(0.,1.,0.));
#16943=DIRECTION('ref_axis',(1.,0.,0.));
#16944=DIRECTION('center_axis',(0.,1.,0.));
#16945=DIRECTION('ref_axis',(1.,0.,0.));
#16946=DIRECTION('',(0.,-1.,0.));
#16947=DIRECTION('center_axis',(0.,1.,0.));
#16948=DIRECTION('ref_axis',(1.,0.,0.));
#16949=DIRECTION('center_axis',(0.,1.,0.));
#16950=DIRECTION('ref_axis',(1.,0.,0.));
#16951=DIRECTION('axis',(0.,0.,1.));
#16952=DIRECTION('refdir',(1.,0.,0.));
#16953=DIRECTION('center_axis',(0.,1.,0.));
#16954=DIRECTION('ref_axis',(1.,0.,0.));
#16955=DIRECTION('center_axis',(0.,1.,0.));
#16956=DIRECTION('ref_axis',(1.,0.,0.));
#16957=DIRECTION('',(0.,1.,0.));
#16958=DIRECTION('center_axis',(0.,-1.,0.));
#16959=DIRECTION('ref_axis',(1.,0.,0.));
#16960=DIRECTION('center_axis',(0.,1.,0.));
#16961=DIRECTION('ref_axis',(1.,0.,0.));
#16962=DIRECTION('center_axis',(0.,1.,0.));
#16963=DIRECTION('ref_axis',(1.,0.,0.));
#16964=DIRECTION('center_axis',(0.,1.,0.));
#16965=DIRECTION('ref_axis',(1.,0.,0.));
#16966=DIRECTION('',(0.,-1.,0.));
#16967=DIRECTION('center_axis',(0.,-1.,0.));
#16968=DIRECTION('ref_axis',(1.,0.,0.));
#16969=DIRECTION('center_axis',(0.,1.,0.));
#16970=DIRECTION('ref_axis',(1.,0.,0.));
#16971=DIRECTION('center_axis',(0.,1.,0.));
#16972=DIRECTION('ref_axis',(1.,0.,0.));
#16973=DIRECTION('',(0.,-1.,0.));
#16974=DIRECTION('center_axis',(0.,1.,0.));
#16975=DIRECTION('ref_axis',(1.,0.,0.));
#16976=DIRECTION('center_axis',(0.,1.,0.));
#16977=DIRECTION('ref_axis',(1.,0.,0.));
#16978=DIRECTION('center_axis',(0.,1.,0.));
#16979=DIRECTION('ref_axis',(1.,0.,0.));
#16980=DIRECTION('axis',(0.,0.,1.));
#16981=DIRECTION('refdir',(1.,0.,0.));
#16982=DIRECTION('center_axis',(0.,1.,0.));
#16983=DIRECTION('ref_axis',(1.,0.,0.));
#16984=DIRECTION('center_axis',(0.,-1.,0.));
#16985=DIRECTION('ref_axis',(1.,0.,0.));
#16986=DIRECTION('',(0.,-1.,0.));
#16987=DIRECTION('center_axis',(0.,-1.,0.));
#16988=DIRECTION('ref_axis',(1.,0.,0.));
#16989=DIRECTION('center_axis',(0.,1.,0.));
#16990=DIRECTION('ref_axis',(1.,0.,0.));
#16991=DIRECTION('center_axis',(0.,1.,0.));
#16992=DIRECTION('ref_axis',(1.,0.,0.));
#16993=DIRECTION('',(0.,-1.,0.));
#16994=DIRECTION('center_axis',(0.,1.,0.));
#16995=DIRECTION('ref_axis',(1.,0.,0.));
#16996=DIRECTION('center_axis',(0.,1.,0.));
#16997=DIRECTION('ref_axis',(1.,0.,0.));
#16998=DIRECTION('center_axis',(0.,1.,0.));
#16999=DIRECTION('ref_axis',(1.,0.,0.));
#17000=DIRECTION('axis',(0.,0.,1.));
#17001=DIRECTION('refdir',(1.,0.,0.));
#17002=DIRECTION('center_axis',(0.,0.,1.));
#17003=DIRECTION('ref_axis',(1.,0.,0.));
#17004=DIRECTION('center_axis',(0.,0.,1.));
#17005=DIRECTION('ref_axis',(1.,0.,0.));
#17006=DIRECTION('',(0.,0.,-1.));
#17007=DIRECTION('center_axis',(0.,0.,1.));
#17008=DIRECTION('ref_axis',(1.,0.,0.));
#17009=DIRECTION('center_axis',(0.,0.,1.));
#17010=DIRECTION('ref_axis',(1.,0.,0.));
#17011=DIRECTION('center_axis',(0.,0.,1.));
#17012=DIRECTION('ref_axis',(1.,0.,0.));
#17013=DIRECTION('axis',(0.,0.,1.));
#17014=DIRECTION('refdir',(1.,0.,0.));
#17015=DIRECTION('center_axis',(0.,0.,1.));
#17016=DIRECTION('ref_axis',(1.,0.,0.));
#17017=DIRECTION('center_axis',(0.,0.,1.));
#17018=DIRECTION('ref_axis',(1.,0.,0.));
#17019=DIRECTION('',(0.,0.,-1.));
#17020=DIRECTION('center_axis',(0.,0.,1.));
#17021=DIRECTION('ref_axis',(1.,0.,0.));
#17022=DIRECTION('center_axis',(0.,0.,1.));
#17023=DIRECTION('ref_axis',(1.,0.,0.));
#17024=DIRECTION('center_axis',(0.,0.,1.));
#17025=DIRECTION('ref_axis',(1.,0.,0.));
#17026=DIRECTION('axis',(0.,0.,1.));
#17027=DIRECTION('refdir',(1.,0.,0.));
#17028=DIRECTION('center_axis',(0.,1.,0.));
#17029=DIRECTION('ref_axis',(1.,0.,0.));
#17030=DIRECTION('center_axis',(0.,-1.,0.));
#17031=DIRECTION('ref_axis',(1.,0.,0.));
#17032=DIRECTION('',(0.,-1.,0.));
#17033=DIRECTION('center_axis',(0.,-1.,0.));
#17034=DIRECTION('ref_axis',(1.,0.,0.));
#17035=DIRECTION('center_axis',(0.,1.,0.));
#17036=DIRECTION('ref_axis',(1.,0.,0.));
#17037=DIRECTION('center_axis',(0.,1.,0.));
#17038=DIRECTION('ref_axis',(1.,0.,0.));
#17039=DIRECTION('',(0.,-1.,0.));
#17040=DIRECTION('center_axis',(0.,1.,0.));
#17041=DIRECTION('ref_axis',(1.,0.,0.));
#17042=DIRECTION('center_axis',(0.,1.,0.));
#17043=DIRECTION('ref_axis',(1.,0.,0.));
#17044=DIRECTION('center_axis',(0.,1.,0.));
#17045=DIRECTION('ref_axis',(1.,0.,0.));
#17046=DIRECTION('axis',(0.,0.,1.));
#17047=DIRECTION('refdir',(1.,0.,0.));
#17048=DIRECTION('center_axis',(1.,0.,6.12323399573677E-17));
#17049=DIRECTION('ref_axis',(6.12323399573677E-17,0.,-1.));
#17050=DIRECTION('',(1.,0.,6.12323399573677E-17));
#17051=DIRECTION('center_axis',(1.,0.,6.12323399573677E-17));
#17052=DIRECTION('ref_axis',(6.12323399573677E-17,0.,-1.));
#17053=DIRECTION('',(1.,0.,6.12323399573677E-17));
#17054=DIRECTION('center_axis',(0.,-1.,0.));
#17055=DIRECTION('ref_axis',(1.,0.,0.));
#17056=DIRECTION('center_axis',(0.,-1.,0.));
#17057=DIRECTION('ref_axis',(1.,0.,0.));
#17058=DIRECTION('',(0.,1.,0.));
#17059=DIRECTION('',(0.,1.,0.));
#17060=DIRECTION('center_axis',(0.,1.,0.));
#17061=DIRECTION('ref_axis',(1.,0.,0.));
#17062=DIRECTION('center_axis',(0.,0.,1.));
#17063=DIRECTION('ref_axis',(1.,0.,0.));
#17064=DIRECTION('',(0.,0.,1.));
#17065=DIRECTION('center_axis',(0.,0.,1.));
#17066=DIRECTION('ref_axis',(1.,0.,0.));
#17067=DIRECTION('',(0.,0.,1.));
#17068=DIRECTION('center_axis',(0.,1.,0.));
#17069=DIRECTION('ref_axis',(1.,0.,0.));
#17070=DIRECTION('center_axis',(0.,1.,0.));
#17071=DIRECTION('ref_axis',(1.,0.,0.));
#17072=DIRECTION('',(0.,1.,0.));
#17073=DIRECTION('',(0.,1.,0.));
#17074=DIRECTION('center_axis',(0.,-1.,0.));
#17075=DIRECTION('ref_axis',(1.,0.,0.));
#17076=DIRECTION('center_axis',(0.,1.,0.));
#17077=DIRECTION('ref_axis',(1.,0.,0.));
#17078=DIRECTION('center_axis',(0.,1.,0.));
#17079=DIRECTION('ref_axis',(1.,0.,0.));
#17080=DIRECTION('center_axis',(0.,1.,0.));
#17081=DIRECTION('ref_axis',(1.,0.,0.));
#17082=DIRECTION('center_axis',(0.,1.,0.));
#17083=DIRECTION('ref_axis',(0.951056516295154,0.,0.309016994374948));
#17084=DIRECTION('center_axis',(0.,1.,0.));
#17085=DIRECTION('ref_axis',(1.,0.,0.));
#17086=DIRECTION('center_axis',(0.,1.,0.));
#17087=DIRECTION('ref_axis',(0.809016994374947,0.,0.587785252292473));
#17088=DIRECTION('center_axis',(0.,1.,0.));
#17089=DIRECTION('ref_axis',(1.,0.,0.));
#17090=DIRECTION('center_axis',(0.,1.,0.));
#17091=DIRECTION('ref_axis',(0.587785252292473,0.,0.809016994374948));
#17092=DIRECTION('center_axis',(0.,1.,0.));
#17093=DIRECTION('ref_axis',(1.,0.,0.));
#17094=DIRECTION('center_axis',(0.,1.,0.));
#17095=DIRECTION('ref_axis',(0.309016994374947,0.,0.951056516295154));
#17096=DIRECTION('center_axis',(0.,1.,0.));
#17097=DIRECTION('ref_axis',(1.,0.,0.));
#17098=DIRECTION('center_axis',(0.,1.,0.));
#17099=DIRECTION('ref_axis',(-1.83697019872103E-16,0.,1.));
#17100=DIRECTION('center_axis',(0.,1.,0.));
#17101=DIRECTION('ref_axis',(1.,0.,0.));
#17102=DIRECTION('center_axis',(0.,1.,0.));
#17103=DIRECTION('ref_axis',(-0.309016994374948,0.,0.951056516295154));
#17104=DIRECTION('center_axis',(0.,1.,0.));
#17105=DIRECTION('ref_axis',(1.,0.,0.));
#17106=DIRECTION('center_axis',(0.,1.,0.));
#17107=DIRECTION('ref_axis',(-0.587785252292473,0.,0.809016994374947));
#17108=DIRECTION('center_axis',(0.,1.,0.));
#17109=DIRECTION('ref_axis',(1.,0.,0.));
#17110=DIRECTION('center_axis',(0.,1.,0.));
#17111=DIRECTION('ref_axis',(-0.809016994374947,0.,0.587785252292473));
#17112=DIRECTION('center_axis',(0.,1.,0.));
#17113=DIRECTION('ref_axis',(1.,0.,0.));
#17114=DIRECTION('center_axis',(0.,1.,0.));
#17115=DIRECTION('ref_axis',(-0.951056516295154,0.,0.309016994374947));
#17116=DIRECTION('center_axis',(0.,1.,0.));
#17117=DIRECTION('ref_axis',(1.,0.,0.));
#17118=DIRECTION('center_axis',(0.,1.,0.));
#17119=DIRECTION('ref_axis',(-1.,0.,-1.22464679914735E-16));
#17120=DIRECTION('center_axis',(0.,1.,0.));
#17121=DIRECTION('ref_axis',(1.,0.,0.));
#17122=DIRECTION('center_axis',(0.,1.,0.));
#17123=DIRECTION('ref_axis',(-0.951056516295154,0.,-0.309016994374948));
#17124=DIRECTION('center_axis',(0.,1.,0.));
#17125=DIRECTION('ref_axis',(1.,0.,0.));
#17126=DIRECTION('center_axis',(0.,1.,0.));
#17127=DIRECTION('ref_axis',(-0.809016994374947,0.,-0.587785252292473));
#17128=DIRECTION('center_axis',(0.,1.,0.));
#17129=DIRECTION('ref_axis',(1.,0.,0.));
#17130=DIRECTION('center_axis',(0.,1.,0.));
#17131=DIRECTION('ref_axis',(-0.587785252292473,0.,-0.809016994374948));
#17132=DIRECTION('center_axis',(0.,1.,0.));
#17133=DIRECTION('ref_axis',(1.,0.,0.));
#17134=DIRECTION('center_axis',(0.,1.,0.));
#17135=DIRECTION('ref_axis',(-0.309016994374947,0.,-0.951056516295154));
#17136=DIRECTION('center_axis',(0.,1.,0.));
#17137=DIRECTION('ref_axis',(1.,0.,0.));
#17138=DIRECTION('center_axis',(0.,1.,0.));
#17139=DIRECTION('ref_axis',(6.12323399573677E-17,0.,-1.));
#17140=DIRECTION('center_axis',(0.,1.,0.));
#17141=DIRECTION('ref_axis',(1.,0.,0.));
#17142=DIRECTION('center_axis',(0.,1.,0.));
#17143=DIRECTION('ref_axis',(0.309016994374947,0.,-0.951056516295154));
#17144=DIRECTION('center_axis',(0.,1.,0.));
#17145=DIRECTION('ref_axis',(1.,0.,0.));
#17146=DIRECTION('center_axis',(0.,1.,0.));
#17147=DIRECTION('ref_axis',(0.587785252292473,0.,-0.809016994374947));
#17148=DIRECTION('center_axis',(0.,1.,0.));
#17149=DIRECTION('ref_axis',(1.,0.,0.));
#17150=DIRECTION('center_axis',(0.,1.,0.));
#17151=DIRECTION('ref_axis',(0.809016994374947,0.,-0.587785252292473));
#17152=DIRECTION('center_axis',(0.,1.,0.));
#17153=DIRECTION('ref_axis',(1.,0.,0.));
#17154=DIRECTION('center_axis',(0.,1.,0.));
#17155=DIRECTION('ref_axis',(0.951056516295154,0.,-0.309016994374947));
#17156=DIRECTION('center_axis',(0.,1.,0.));
#17157=DIRECTION('ref_axis',(1.,0.,0.));
#17158=DIRECTION('center_axis',(0.,1.,0.));
#17159=DIRECTION('ref_axis',(1.,0.,0.));
#17160=DIRECTION('center_axis',(0.,1.,0.));
#17161=DIRECTION('ref_axis',(1.,0.,0.));
#17162=DIRECTION('center_axis',(0.,-1.,0.));
#17163=DIRECTION('ref_axis',(1.,0.,0.));
#17164=DIRECTION('center_axis',(0.,-1.,0.));
#17165=DIRECTION('ref_axis',(1.,0.,0.));
#17166=DIRECTION('',(0.,1.,0.));
#17167=DIRECTION('center_axis',(0.,1.,0.));
#17168=DIRECTION('ref_axis',(1.,0.,0.));
#17169=DIRECTION('center_axis',(0.,1.,0.));
#17170=DIRECTION('ref_axis',(1.,0.,0.));
#17171=DIRECTION('center_axis',(0.,1.,0.));
#17172=DIRECTION('ref_axis',(1.,0.,0.));
#17173=DIRECTION('center_axis',(0.,-1.,0.));
#17174=DIRECTION('ref_axis',(0.951056516295154,0.,0.309016994374948));
#17175=DIRECTION('center_axis',(0.,1.,0.));
#17176=DIRECTION('ref_axis',(1.,0.,0.));
#17177=DIRECTION('center_axis',(0.,-1.,0.));
#17178=DIRECTION('ref_axis',(1.,0.,0.));
#17179=DIRECTION('center_axis',(0.,1.,0.));
#17180=DIRECTION('ref_axis',(1.,0.,0.));
#17181=DIRECTION('center_axis',(0.,-1.,0.));
#17182=DIRECTION('ref_axis',(0.951056516295154,0.,-0.309016994374947));
#17183=DIRECTION('center_axis',(0.,1.,0.));
#17184=DIRECTION('ref_axis',(1.,0.,0.));
#17185=DIRECTION('center_axis',(0.,-1.,0.));
#17186=DIRECTION('ref_axis',(0.809016994374947,0.,-0.587785252292473));
#17187=DIRECTION('center_axis',(0.,1.,0.));
#17188=DIRECTION('ref_axis',(1.,0.,0.));
#17189=DIRECTION('center_axis',(0.,-1.,0.));
#17190=DIRECTION('ref_axis',(0.587785252292473,0.,-0.809016994374947));
#17191=DIRECTION('center_axis',(0.,1.,0.));
#17192=DIRECTION('ref_axis',(1.,0.,0.));
#17193=DIRECTION('center_axis',(0.,-1.,0.));
#17194=DIRECTION('ref_axis',(0.309016994374947,0.,-0.951056516295154));
#17195=DIRECTION('center_axis',(0.,1.,0.));
#17196=DIRECTION('ref_axis',(1.,0.,0.));
#17197=DIRECTION('center_axis',(0.,-1.,0.));
#17198=DIRECTION('ref_axis',(6.12323399573677E-17,0.,-1.));
#17199=DIRECTION('center_axis',(0.,1.,0.));
#17200=DIRECTION('ref_axis',(1.,0.,0.));
#17201=DIRECTION('center_axis',(0.,-1.,0.));
#17202=DIRECTION('ref_axis',(-0.309016994374947,0.,-0.951056516295154));
#17203=DIRECTION('center_axis',(0.,1.,0.));
#17204=DIRECTION('ref_axis',(1.,0.,0.));
#17205=DIRECTION('center_axis',(0.,-1.,0.));
#17206=DIRECTION('ref_axis',(-0.587785252292473,0.,-0.809016994374948));
#17207=DIRECTION('center_axis',(0.,1.,0.));
#17208=DIRECTION('ref_axis',(1.,0.,0.));
#17209=DIRECTION('center_axis',(0.,-1.,0.));
#17210=DIRECTION('ref_axis',(-0.809016994374947,0.,-0.587785252292473));
#17211=DIRECTION('center_axis',(0.,1.,0.));
#17212=DIRECTION('ref_axis',(1.,0.,0.));
#17213=DIRECTION('center_axis',(0.,-1.,0.));
#17214=DIRECTION('ref_axis',(-0.951056516295154,0.,-0.309016994374948));
#17215=DIRECTION('center_axis',(0.,1.,0.));
#17216=DIRECTION('ref_axis',(1.,0.,0.));
#17217=DIRECTION('center_axis',(0.,-1.,0.));
#17218=DIRECTION('ref_axis',(-1.,0.,-1.22464679914735E-16));
#17219=DIRECTION('center_axis',(0.,1.,0.));
#17220=DIRECTION('ref_axis',(1.,0.,0.));
#17221=DIRECTION('center_axis',(0.,-1.,0.));
#17222=DIRECTION('ref_axis',(-0.951056516295154,0.,0.309016994374947));
#17223=DIRECTION('center_axis',(0.,1.,0.));
#17224=DIRECTION('ref_axis',(1.,0.,0.));
#17225=DIRECTION('center_axis',(0.,-1.,0.));
#17226=DIRECTION('ref_axis',(-0.809016994374947,0.,0.587785252292473));
#17227=DIRECTION('center_axis',(0.,1.,0.));
#17228=DIRECTION('ref_axis',(1.,0.,0.));
#17229=DIRECTION('center_axis',(0.,-1.,0.));
#17230=DIRECTION('ref_axis',(-0.587785252292473,0.,0.809016994374947));
#17231=DIRECTION('center_axis',(0.,1.,0.));
#17232=DIRECTION('ref_axis',(1.,0.,0.));
#17233=DIRECTION('center_axis',(0.,-1.,0.));
#17234=DIRECTION('ref_axis',(-0.309016994374948,0.,0.951056516295154));
#17235=DIRECTION('center_axis',(0.,1.,0.));
#17236=DIRECTION('ref_axis',(1.,0.,0.));
#17237=DIRECTION('center_axis',(0.,-1.,0.));
#17238=DIRECTION('ref_axis',(-1.83697019872103E-16,0.,1.));
#17239=DIRECTION('center_axis',(0.,1.,0.));
#17240=DIRECTION('ref_axis',(1.,0.,0.));
#17241=DIRECTION('center_axis',(0.,-1.,0.));
#17242=DIRECTION('ref_axis',(0.309016994374947,0.,0.951056516295154));
#17243=DIRECTION('center_axis',(0.,1.,0.));
#17244=DIRECTION('ref_axis',(1.,0.,0.));
#17245=DIRECTION('center_axis',(0.,-1.,0.));
#17246=DIRECTION('ref_axis',(0.587785252292473,0.,0.809016994374948));
#17247=DIRECTION('center_axis',(0.,1.,0.));
#17248=DIRECTION('ref_axis',(1.,0.,0.));
#17249=DIRECTION('center_axis',(0.,-1.,0.));
#17250=DIRECTION('ref_axis',(0.809016994374947,0.,0.587785252292473));
#17251=DIRECTION('center_axis',(0.,1.,0.));
#17252=DIRECTION('ref_axis',(1.,0.,0.));
#17253=DIRECTION('center_axis',(0.,1.,0.));
#17254=DIRECTION('ref_axis',(1.,0.,0.));
#17255=DIRECTION('center_axis',(0.,1.,0.));
#17256=DIRECTION('ref_axis',(1.,0.,0.));
#17257=DIRECTION('',(0.,-1.,0.));
#17258=DIRECTION('center_axis',(0.,1.,0.));
#17259=DIRECTION('ref_axis',(1.,0.,0.));
#17260=DIRECTION('center_axis',(0.,1.,0.));
#17261=DIRECTION('ref_axis',(-0.951056516295153,0.,-0.309016994374948));
#17262=DIRECTION('',(0.,-1.,0.));
#17263=DIRECTION('',(0.,1.,0.));
#17264=DIRECTION('center_axis',(0.,1.,0.));
#17265=DIRECTION('ref_axis',(1.,0.,0.));
#17266=DIRECTION('',(0.,-1.,0.));
#17267=DIRECTION('center_axis',(0.,1.,0.));
#17268=DIRECTION('ref_axis',(-0.809016994374947,0.,-0.587785252292473));
#17269=DIRECTION('',(0.,1.,0.));
#17270=DIRECTION('center_axis',(0.,1.,0.));
#17271=DIRECTION('ref_axis',(1.,0.,0.));
#17272=DIRECTION('',(0.,-1.,0.));
#17273=DIRECTION('center_axis',(0.,1.,0.));
#17274=DIRECTION('ref_axis',(-0.587785252292473,0.,-0.809016994374947));
#17275=DIRECTION('',(0.,1.,0.));
#17276=DIRECTION('center_axis',(0.,1.,0.));
#17277=DIRECTION('ref_axis',(1.,0.,0.));
#17278=DIRECTION('',(0.,-1.,0.));
#17279=DIRECTION('center_axis',(0.,1.,0.));
#17280=DIRECTION('ref_axis',(-0.309016994374947,0.,-0.951056516295154));
#17281=DIRECTION('',(0.,1.,0.));
#17282=DIRECTION('center_axis',(0.,1.,0.));
#17283=DIRECTION('ref_axis',(1.,0.,0.));
#17284=DIRECTION('',(0.,-1.,0.));
#17285=DIRECTION('center_axis',(0.,1.,0.));
#17286=DIRECTION('ref_axis',(-1.37927510063224E-16,0.,-1.));
#17287=DIRECTION('',(0.,1.,0.));
#17288=DIRECTION('center_axis',(0.,1.,0.));
#17289=DIRECTION('ref_axis',(1.,0.,0.));
#17290=DIRECTION('',(0.,-1.,0.));
#17291=DIRECTION('center_axis',(0.,1.,0.));
#17292=DIRECTION('ref_axis',(0.309016994374948,0.,-0.951056516295154));
#17293=DIRECTION('',(0.,1.,0.));
#17294=DIRECTION('center_axis',(0.,1.,0.));
#17295=DIRECTION('ref_axis',(1.,0.,0.));
#17296=DIRECTION('',(0.,-1.,0.));
#17297=DIRECTION('center_axis',(0.,1.,0.));
#17298=DIRECTION('ref_axis',(0.587785252292473,0.,-0.809016994374948));
#17299=DIRECTION('',(0.,1.,0.));
#17300=DIRECTION('center_axis',(0.,1.,0.));
#17301=DIRECTION('ref_axis',(1.,0.,0.));
#17302=DIRECTION('',(0.,-1.,0.));
#17303=DIRECTION('center_axis',(0.,1.,0.));
#17304=DIRECTION('ref_axis',(0.809016994374948,0.,-0.587785252292473));
#17305=DIRECTION('',(0.,1.,0.));
#17306=DIRECTION('center_axis',(0.,1.,0.));
#17307=DIRECTION('ref_axis',(1.,0.,0.));
#17308=DIRECTION('',(0.,-1.,0.));
#17309=DIRECTION('center_axis',(0.,1.,0.));
#17310=DIRECTION('ref_axis',(0.951056516295154,0.,-0.309016994374947));
#17311=DIRECTION('',(0.,1.,0.));
#17312=DIRECTION('center_axis',(0.,1.,0.));
#17313=DIRECTION('ref_axis',(1.,0.,0.));
#17314=DIRECTION('',(0.,-1.,0.));
#17315=DIRECTION('center_axis',(0.,1.,0.));
#17316=DIRECTION('ref_axis',(1.,0.,-1.99159850020592E-16));
#17317=DIRECTION('',(0.,1.,0.));
#17318=DIRECTION('center_axis',(0.,1.,0.));
#17319=DIRECTION('ref_axis',(1.,0.,0.));
#17320=DIRECTION('',(0.,-1.,0.));
#17321=DIRECTION('center_axis',(0.,1.,0.));
#17322=DIRECTION('ref_axis',(0.951056516295154,0.,0.309016994374948));
#17323=DIRECTION('',(0.,1.,0.));
#17324=DIRECTION('center_axis',(0.,1.,0.));
#17325=DIRECTION('ref_axis',(1.,0.,0.));
#17326=DIRECTION('',(0.,-1.,0.));
#17327=DIRECTION('center_axis',(0.,1.,0.));
#17328=DIRECTION('ref_axis',(0.809016994374948,0.,0.587785252292473));
#17329=DIRECTION('',(0.,1.,0.));
#17330=DIRECTION('center_axis',(0.,1.,0.));
#17331=DIRECTION('ref_axis',(1.,0.,0.));
#17332=DIRECTION('',(0.,-1.,0.));
#17333=DIRECTION('center_axis',(0.,1.,0.));
#17334=DIRECTION('ref_axis',(0.587785252292473,0.,0.809016994374948));
#17335=DIRECTION('',(0.,1.,0.));
#17336=DIRECTION('center_axis',(0.,1.,0.));
#17337=DIRECTION('ref_axis',(1.,0.,0.));
#17338=DIRECTION('',(0.,-1.,0.));
#17339=DIRECTION('center_axis',(0.,1.,0.));
#17340=DIRECTION('ref_axis',(0.309016994374947,0.,0.951056516295154));
#17341=DIRECTION('',(0.,1.,0.));
#17342=DIRECTION('center_axis',(0.,1.,0.));
#17343=DIRECTION('ref_axis',(1.,0.,0.));
#17344=DIRECTION('',(0.,-1.,0.));
#17345=DIRECTION('center_axis',(0.,1.,0.));
#17346=DIRECTION('ref_axis',(2.6039218997796E-16,0.,1.));
#17347=DIRECTION('',(0.,1.,0.));
#17348=DIRECTION('center_axis',(0.,1.,0.));
#17349=DIRECTION('ref_axis',(1.,0.,0.));
#17350=DIRECTION('',(0.,-1.,0.));
#17351=DIRECTION('center_axis',(0.,1.,0.));
#17352=DIRECTION('ref_axis',(-0.309016994374948,0.,0.951056516295153));
#17353=DIRECTION('',(0.,1.,0.));
#17354=DIRECTION('center_axis',(0.,1.,0.));
#17355=DIRECTION('ref_axis',(1.,0.,0.));
#17356=DIRECTION('',(0.,-1.,0.));
#17357=DIRECTION('center_axis',(0.,1.,0.));
#17358=DIRECTION('ref_axis',(-0.587785252292474,0.,0.809016994374947));
#17359=DIRECTION('',(0.,1.,0.));
#17360=DIRECTION('center_axis',(0.,1.,0.));
#17361=DIRECTION('ref_axis',(1.,0.,0.));
#17362=DIRECTION('',(0.,-1.,0.));
#17363=DIRECTION('center_axis',(0.,1.,0.));
#17364=DIRECTION('ref_axis',(-0.809016994374948,0.,0.587785252292473));
#17365=DIRECTION('',(0.,1.,0.));
#17366=DIRECTION('center_axis',(0.,1.,0.));
#17367=DIRECTION('ref_axis',(1.,0.,0.));
#17368=DIRECTION('',(0.,-1.,0.));
#17369=DIRECTION('center_axis',(0.,1.,0.));
#17370=DIRECTION('ref_axis',(-0.951056516295154,0.,0.309016994374948));
#17371=DIRECTION('',(0.,1.,0.));
#17372=DIRECTION('center_axis',(0.,1.,0.));
#17373=DIRECTION('ref_axis',(1.,0.,0.));
#17374=DIRECTION('',(0.,1.,0.));
#17375=DIRECTION('center_axis',(0.,1.,0.));
#17376=DIRECTION('ref_axis',(-1.,0.,-1.22464679914735E-16));
#17377=DIRECTION('',(0.,-1.,0.));
#17378=DIRECTION('center_axis',(0.,1.,0.));
#17379=DIRECTION('ref_axis',(1.,0.,0.));
#17380=DIRECTION('axis',(0.,0.,1.));
#17381=DIRECTION('refdir',(1.,0.,0.));
#17382=DIRECTION('axis',(0.,0.,1.));
#17383=DIRECTION('refdir',(1.,0.,0.));
#17384=DIRECTION('center_axis',(0.,1.,0.));
#17385=DIRECTION('ref_axis',(1.,0.,0.));
#17386=DIRECTION('center_axis',(0.,1.,0.));
#17387=DIRECTION('ref_axis',(1.,0.,0.));
#17388=DIRECTION('',(0.,1.,0.));
#17389=DIRECTION('center_axis',(0.,1.,0.));
#17390=DIRECTION('ref_axis',(1.,0.,0.));
#17391=DIRECTION('center_axis',(0.,1.,0.));
#17392=DIRECTION('ref_axis',(1.,0.,0.));
#17393=DIRECTION('center_axis',(0.,1.,0.));
#17394=DIRECTION('ref_axis',(1.,0.,0.));
#17395=DIRECTION('center_axis',(0.,1.,0.));
#17396=DIRECTION('ref_axis',(1.,0.,0.));
#17397=DIRECTION('center_axis',(0.,1.,0.));
#17398=DIRECTION('ref_axis',(1.,0.,0.));
#17399=DIRECTION('center_axis',(0.,1.,0.));
#17400=DIRECTION('ref_axis',(1.,0.,0.));
#17401=DIRECTION('center_axis',(0.,1.,0.));
#17402=DIRECTION('ref_axis',(1.,0.,0.));
#17403=DIRECTION('center_axis',(0.,-1.,0.));
#17404=DIRECTION('ref_axis',(1.,0.,0.));
#17405=DIRECTION('center_axis',(0.,1.,0.));
#17406=DIRECTION('ref_axis',(1.,0.,0.));
#17407=DIRECTION('',(0.,-1.,0.));
#17408=DIRECTION('center_axis',(0.,1.,0.));
#17409=DIRECTION('ref_axis',(1.,0.,0.));
#17410=DIRECTION('',(0.,-1.,0.));
#17411=DIRECTION('center_axis',(0.,1.,0.));
#17412=DIRECTION('ref_axis',(1.,0.,0.));
#17413=DIRECTION('center_axis',(0.,1.,0.));
#17414=DIRECTION('ref_axis',(1.,0.,0.));
#17415=DIRECTION('center_axis',(0.,1.,0.));
#17416=DIRECTION('ref_axis',(1.,0.,0.));
#17417=DIRECTION('center_axis',(0.,1.,0.));
#17418=DIRECTION('ref_axis',(1.,0.,0.));
#17419=DIRECTION('',(0.,-1.,0.));
#17420=DIRECTION('center_axis',(0.,1.,0.));
#17421=DIRECTION('ref_axis',(1.,0.,0.));
#17422=DIRECTION('axis',(0.,0.,1.));
#17423=DIRECTION('refdir',(1.,0.,0.));
#17424=DIRECTION('center_axis',(0.,1.,0.));
#17425=DIRECTION('ref_axis',(1.,0.,0.));
#17426=DIRECTION('center_axis',(0.,-1.,0.));
#17427=DIRECTION('ref_axis',(1.,0.,0.));
#17428=DIRECTION('',(0.,-1.,0.));
#17429=DIRECTION('center_axis',(0.,-1.,0.));
#17430=DIRECTION('ref_axis',(1.,0.,0.));
#17431=DIRECTION('center_axis',(0.,1.,0.));
#17432=DIRECTION('ref_axis',(1.,0.,0.));
#17433=DIRECTION('center_axis',(0.,1.,0.));
#17434=DIRECTION('ref_axis',(1.,0.,0.));
#17435=DIRECTION('',(0.,-1.,0.));
#17436=DIRECTION('center_axis',(0.,1.,0.));
#17437=DIRECTION('ref_axis',(1.,0.,0.));
#17438=DIRECTION('center_axis',(0.,1.,0.));
#17439=DIRECTION('ref_axis',(1.,0.,0.));
#17440=DIRECTION('center_axis',(0.,1.,0.));
#17441=DIRECTION('ref_axis',(1.,0.,0.));
#17442=DIRECTION('axis',(0.,0.,1.));
#17443=DIRECTION('refdir',(1.,0.,0.));
#17444=DIRECTION('center_axis',(0.,1.,0.));
#17445=DIRECTION('ref_axis',(1.,0.,0.));
#17446=DIRECTION('center_axis',(0.,-1.,0.));
#17447=DIRECTION('ref_axis',(1.,0.,0.));
#17448=DIRECTION('',(0.,-1.,0.));
#17449=DIRECTION('center_axis',(0.,-1.,0.));
#17450=DIRECTION('ref_axis',(1.,0.,0.));
#17451=DIRECTION('center_axis',(0.,1.,0.));
#17452=DIRECTION('ref_axis',(1.,0.,0.));
#17453=DIRECTION('center_axis',(0.,1.,0.));
#17454=DIRECTION('ref_axis',(1.,0.,0.));
#17455=DIRECTION('',(0.,-1.,0.));
#17456=DIRECTION('center_axis',(0.,1.,0.));
#17457=DIRECTION('ref_axis',(1.,0.,0.));
#17458=DIRECTION('center_axis',(0.,1.,0.));
#17459=DIRECTION('ref_axis',(1.,0.,0.));
#17460=DIRECTION('center_axis',(0.,1.,0.));
#17461=DIRECTION('ref_axis',(1.,0.,0.));
#17462=DIRECTION('axis',(0.,0.,1.));
#17463=DIRECTION('refdir',(1.,0.,0.));
#17464=DIRECTION('center_axis',(0.,0.,1.));
#17465=DIRECTION('ref_axis',(1.,0.,0.));
#17466=DIRECTION('center_axis',(0.,0.,1.));
#17467=DIRECTION('ref_axis',(1.,0.,0.));
#17468=DIRECTION('',(0.,0.,-1.));
#17469=DIRECTION('center_axis',(0.,0.,1.));
#17470=DIRECTION('ref_axis',(1.,0.,0.));
#17471=DIRECTION('center_axis',(0.,0.,1.));
#17472=DIRECTION('ref_axis',(1.,0.,0.));
#17473=DIRECTION('center_axis',(0.,0.,1.));
#17474=DIRECTION('ref_axis',(1.,0.,0.));
#17475=DIRECTION('axis',(0.,0.,1.));
#17476=DIRECTION('refdir',(1.,0.,0.));
#17477=DIRECTION('center_axis',(0.,0.,1.));
#17478=DIRECTION('ref_axis',(1.,0.,0.));
#17479=DIRECTION('center_axis',(0.,0.,1.));
#17480=DIRECTION('ref_axis',(1.,0.,0.));
#17481=DIRECTION('',(0.,0.,-1.));
#17482=DIRECTION('center_axis',(0.,0.,1.));
#17483=DIRECTION('ref_axis',(1.,0.,0.));
#17484=DIRECTION('center_axis',(0.,0.,1.));
#17485=DIRECTION('ref_axis',(1.,0.,0.));
#17486=DIRECTION('center_axis',(0.,0.,1.));
#17487=DIRECTION('ref_axis',(1.,0.,0.));
#17488=DIRECTION('axis',(0.,0.,1.));
#17489=DIRECTION('refdir',(1.,0.,0.));
#17490=DIRECTION('center_axis',(0.,1.,0.));
#17491=DIRECTION('ref_axis',(1.,0.,0.));
#17492=DIRECTION('center_axis',(0.,-1.,0.));
#17493=DIRECTION('ref_axis',(1.,0.,0.));
#17494=DIRECTION('',(0.,-1.,0.));
#17495=DIRECTION('center_axis',(0.,-1.,0.));
#17496=DIRECTION('ref_axis',(1.,0.,0.));
#17497=DIRECTION('center_axis',(0.,1.,0.));
#17498=DIRECTION('ref_axis',(1.,0.,0.));
#17499=DIRECTION('center_axis',(0.,1.,0.));
#17500=DIRECTION('ref_axis',(1.,0.,0.));
#17501=DIRECTION('',(0.,-1.,0.));
#17502=DIRECTION('center_axis',(0.,1.,0.));
#17503=DIRECTION('ref_axis',(1.,0.,0.));
#17504=DIRECTION('center_axis',(0.,1.,0.));
#17505=DIRECTION('ref_axis',(1.,0.,0.));
#17506=DIRECTION('center_axis',(0.,1.,0.));
#17507=DIRECTION('ref_axis',(1.,0.,0.));
#17508=DIRECTION('axis',(0.,0.,1.));
#17509=DIRECTION('refdir',(1.,0.,0.));
#17510=DIRECTION('center_axis',(1.,0.,6.12323399573677E-17));
#17511=DIRECTION('ref_axis',(6.12323399573677E-17,0.,-1.));
#17512=DIRECTION('',(1.,0.,6.12323399573677E-17));
#17513=DIRECTION('center_axis',(1.,0.,6.12323399573677E-17));
#17514=DIRECTION('ref_axis',(6.12323399573677E-17,0.,-1.));
#17515=DIRECTION('',(1.,0.,6.12323399573677E-17));
#17516=DIRECTION('center_axis',(0.,-1.,0.));
#17517=DIRECTION('ref_axis',(1.,0.,0.));
#17518=DIRECTION('center_axis',(0.,-1.,0.));
#17519=DIRECTION('ref_axis',(1.,0.,0.));
#17520=DIRECTION('',(0.,1.,0.));
#17521=DIRECTION('',(0.,1.,0.));
#17522=DIRECTION('center_axis',(0.,1.,0.));
#17523=DIRECTION('ref_axis',(1.,0.,0.));
#17524=DIRECTION('center_axis',(0.,0.,1.));
#17525=DIRECTION('ref_axis',(1.,0.,0.));
#17526=DIRECTION('',(0.,0.,1.));
#17527=DIRECTION('center_axis',(0.,0.,1.));
#17528=DIRECTION('ref_axis',(1.,0.,0.));
#17529=DIRECTION('',(0.,0.,1.));
#17530=DIRECTION('center_axis',(0.,1.,0.));
#17531=DIRECTION('ref_axis',(1.,0.,0.));
#17532=DIRECTION('center_axis',(0.,1.,0.));
#17533=DIRECTION('ref_axis',(1.,0.,0.));
#17534=DIRECTION('',(0.,1.,0.));
#17535=DIRECTION('',(0.,1.,0.));
#17536=DIRECTION('center_axis',(0.,-1.,0.));
#17537=DIRECTION('ref_axis',(1.,0.,0.));
#17538=DIRECTION('center_axis',(0.,1.,0.));
#17539=DIRECTION('ref_axis',(1.,0.,0.));
#17540=DIRECTION('center_axis',(0.,1.,0.));
#17541=DIRECTION('ref_axis',(1.,0.,0.));
#17542=DIRECTION('center_axis',(0.,1.,0.));
#17543=DIRECTION('ref_axis',(1.,0.,0.));
#17544=DIRECTION('center_axis',(0.,1.,0.));
#17545=DIRECTION('ref_axis',(0.987688340595138,0.,0.156434465040231));
#17546=DIRECTION('center_axis',(0.,1.,0.));
#17547=DIRECTION('ref_axis',(1.,0.,0.));
#17548=DIRECTION('center_axis',(0.,1.,0.));
#17549=DIRECTION('ref_axis',(0.951056516295154,0.,0.309016994374948));
#17550=DIRECTION('center_axis',(0.,1.,0.));
#17551=DIRECTION('ref_axis',(1.,0.,0.));
#17552=DIRECTION('center_axis',(0.,1.,0.));
#17553=DIRECTION('ref_axis',(0.891006524188368,0.,0.453990499739547));
#17554=DIRECTION('center_axis',(0.,1.,0.));
#17555=DIRECTION('ref_axis',(1.,0.,0.));
#17556=DIRECTION('center_axis',(0.,1.,0.));
#17557=DIRECTION('ref_axis',(0.809016994374947,0.,0.587785252292473));
#17558=DIRECTION('center_axis',(0.,1.,0.));
#17559=DIRECTION('ref_axis',(1.,0.,0.));
#17560=DIRECTION('center_axis',(0.,1.,0.));
#17561=DIRECTION('ref_axis',(0.707106781186547,0.,0.707106781186548));
#17562=DIRECTION('center_axis',(0.,1.,0.));
#17563=DIRECTION('ref_axis',(1.,0.,0.));
#17564=DIRECTION('center_axis',(0.,1.,0.));
#17565=DIRECTION('ref_axis',(0.587785252292473,0.,0.809016994374948));
#17566=DIRECTION('center_axis',(0.,1.,0.));
#17567=DIRECTION('ref_axis',(1.,0.,0.));
#17568=DIRECTION('center_axis',(0.,1.,0.));
#17569=DIRECTION('ref_axis',(0.453990499739547,0.,0.891006524188368));
#17570=DIRECTION('center_axis',(0.,1.,0.));
#17571=DIRECTION('ref_axis',(1.,0.,0.));
#17572=DIRECTION('center_axis',(0.,1.,0.));
#17573=DIRECTION('ref_axis',(0.309016994374947,0.,0.951056516295154));
#17574=DIRECTION('center_axis',(0.,1.,0.));
#17575=DIRECTION('ref_axis',(1.,0.,0.));
#17576=DIRECTION('center_axis',(0.,1.,0.));
#17577=DIRECTION('ref_axis',(0.156434465040231,0.,0.987688340595138));
#17578=DIRECTION('center_axis',(0.,1.,0.));
#17579=DIRECTION('ref_axis',(1.,0.,0.));
#17580=DIRECTION('center_axis',(0.,1.,0.));
#17581=DIRECTION('ref_axis',(-1.83697019872103E-16,0.,1.));
#17582=DIRECTION('center_axis',(0.,1.,0.));
#17583=DIRECTION('ref_axis',(1.,0.,0.));
#17584=DIRECTION('center_axis',(0.,1.,0.));
#17585=DIRECTION('ref_axis',(-0.156434465040231,0.,0.987688340595138));
#17586=DIRECTION('center_axis',(0.,1.,0.));
#17587=DIRECTION('ref_axis',(1.,0.,0.));
#17588=DIRECTION('center_axis',(0.,1.,0.));
#17589=DIRECTION('ref_axis',(-0.309016994374948,0.,0.951056516295154));
#17590=DIRECTION('center_axis',(0.,1.,0.));
#17591=DIRECTION('ref_axis',(1.,0.,0.));
#17592=DIRECTION('center_axis',(0.,1.,0.));
#17593=DIRECTION('ref_axis',(-0.453990499739547,0.,0.891006524188368));
#17594=DIRECTION('center_axis',(0.,1.,0.));
#17595=DIRECTION('ref_axis',(1.,0.,0.));
#17596=DIRECTION('center_axis',(0.,1.,0.));
#17597=DIRECTION('ref_axis',(-0.587785252292473,0.,0.809016994374947));
#17598=DIRECTION('center_axis',(0.,1.,0.));
#17599=DIRECTION('ref_axis',(1.,0.,0.));
#17600=DIRECTION('center_axis',(0.,1.,0.));
#17601=DIRECTION('ref_axis',(-0.707106781186548,0.,0.707106781186547));
#17602=DIRECTION('center_axis',(0.,1.,0.));
#17603=DIRECTION('ref_axis',(1.,0.,0.));
#17604=DIRECTION('center_axis',(0.,1.,0.));
#17605=DIRECTION('ref_axis',(-0.809016994374947,0.,0.587785252292473));
#17606=DIRECTION('center_axis',(0.,1.,0.));
#17607=DIRECTION('ref_axis',(1.,0.,0.));
#17608=DIRECTION('center_axis',(0.,1.,0.));
#17609=DIRECTION('ref_axis',(-0.891006524188368,0.,0.453990499739547));
#17610=DIRECTION('center_axis',(0.,1.,0.));
#17611=DIRECTION('ref_axis',(1.,0.,0.));
#17612=DIRECTION('center_axis',(0.,1.,0.));
#17613=DIRECTION('ref_axis',(-0.951056516295154,0.,0.309016994374947));
#17614=DIRECTION('center_axis',(0.,1.,0.));
#17615=DIRECTION('ref_axis',(1.,0.,0.));
#17616=DIRECTION('center_axis',(0.,1.,0.));
#17617=DIRECTION('ref_axis',(-0.987688340595138,0.,0.156434465040231));
#17618=DIRECTION('center_axis',(0.,1.,0.));
#17619=DIRECTION('ref_axis',(1.,0.,0.));
#17620=DIRECTION('center_axis',(0.,1.,0.));
#17621=DIRECTION('ref_axis',(-1.,0.,-1.22464679914735E-16));
#17622=DIRECTION('center_axis',(0.,1.,0.));
#17623=DIRECTION('ref_axis',(1.,0.,0.));
#17624=DIRECTION('center_axis',(0.,1.,0.));
#17625=DIRECTION('ref_axis',(-0.987688340595138,0.,-0.156434465040231));
#17626=DIRECTION('center_axis',(0.,1.,0.));
#17627=DIRECTION('ref_axis',(1.,0.,0.));
#17628=DIRECTION('center_axis',(0.,1.,0.));
#17629=DIRECTION('ref_axis',(-0.951056516295154,0.,-0.309016994374948));
#17630=DIRECTION('center_axis',(0.,1.,0.));
#17631=DIRECTION('ref_axis',(1.,0.,0.));
#17632=DIRECTION('center_axis',(0.,1.,0.));
#17633=DIRECTION('ref_axis',(-0.891006524188368,0.,-0.453990499739547));
#17634=DIRECTION('center_axis',(0.,1.,0.));
#17635=DIRECTION('ref_axis',(1.,0.,0.));
#17636=DIRECTION('center_axis',(0.,1.,0.));
#17637=DIRECTION('ref_axis',(-0.809016994374947,0.,-0.587785252292473));
#17638=DIRECTION('center_axis',(0.,1.,0.));
#17639=DIRECTION('ref_axis',(1.,0.,0.));
#17640=DIRECTION('center_axis',(0.,1.,0.));
#17641=DIRECTION('ref_axis',(-0.707106781186547,0.,-0.707106781186548));
#17642=DIRECTION('center_axis',(0.,1.,0.));
#17643=DIRECTION('ref_axis',(1.,0.,0.));
#17644=DIRECTION('center_axis',(0.,1.,0.));
#17645=DIRECTION('ref_axis',(-0.587785252292473,0.,-0.809016994374947));
#17646=DIRECTION('center_axis',(0.,1.,0.));
#17647=DIRECTION('ref_axis',(1.,0.,0.));
#17648=DIRECTION('center_axis',(0.,1.,0.));
#17649=DIRECTION('ref_axis',(-0.453990499739547,0.,-0.891006524188368));
#17650=DIRECTION('center_axis',(0.,1.,0.));
#17651=DIRECTION('ref_axis',(1.,0.,0.));
#17652=DIRECTION('center_axis',(0.,1.,0.));
#17653=DIRECTION('ref_axis',(-0.309016994374947,0.,-0.951056516295154));
#17654=DIRECTION('center_axis',(0.,1.,0.));
#17655=DIRECTION('ref_axis',(1.,0.,0.));
#17656=DIRECTION('center_axis',(0.,1.,0.));
#17657=DIRECTION('ref_axis',(-0.156434465040231,0.,-0.987688340595138));
#17658=DIRECTION('center_axis',(0.,1.,0.));
#17659=DIRECTION('ref_axis',(1.,0.,0.));
#17660=DIRECTION('center_axis',(0.,1.,0.));
#17661=DIRECTION('ref_axis',(6.12323399573677E-17,0.,-1.));
#17662=DIRECTION('center_axis',(0.,1.,0.));
#17663=DIRECTION('ref_axis',(1.,0.,0.));
#17664=DIRECTION('center_axis',(0.,1.,0.));
#17665=DIRECTION('ref_axis',(0.156434465040231,0.,-0.987688340595138));
#17666=DIRECTION('center_axis',(0.,1.,0.));
#17667=DIRECTION('ref_axis',(1.,0.,0.));
#17668=DIRECTION('center_axis',(0.,1.,0.));
#17669=DIRECTION('ref_axis',(0.309016994374948,0.,-0.951056516295154));
#17670=DIRECTION('center_axis',(0.,1.,0.));
#17671=DIRECTION('ref_axis',(1.,0.,0.));
#17672=DIRECTION('center_axis',(0.,1.,0.));
#17673=DIRECTION('ref_axis',(0.453990499739547,0.,-0.891006524188368));
#17674=DIRECTION('center_axis',(0.,1.,0.));
#17675=DIRECTION('ref_axis',(1.,0.,0.));
#17676=DIRECTION('center_axis',(0.,1.,0.));
#17677=DIRECTION('ref_axis',(0.587785252292473,0.,-0.809016994374947));
#17678=DIRECTION('center_axis',(0.,1.,0.));
#17679=DIRECTION('ref_axis',(1.,0.,0.));
#17680=DIRECTION('center_axis',(0.,1.,0.));
#17681=DIRECTION('ref_axis',(0.707106781186548,0.,-0.707106781186547));
#17682=DIRECTION('center_axis',(0.,1.,0.));
#17683=DIRECTION('ref_axis',(1.,0.,0.));
#17684=DIRECTION('center_axis',(0.,1.,0.));
#17685=DIRECTION('ref_axis',(0.809016994374947,0.,-0.587785252292473));
#17686=DIRECTION('center_axis',(0.,1.,0.));
#17687=DIRECTION('ref_axis',(1.,0.,0.));
#17688=DIRECTION('center_axis',(0.,1.,0.));
#17689=DIRECTION('ref_axis',(0.891006524188368,0.,-0.453990499739547));
#17690=DIRECTION('center_axis',(0.,1.,0.));
#17691=DIRECTION('ref_axis',(1.,0.,0.));
#17692=DIRECTION('center_axis',(0.,1.,0.));
#17693=DIRECTION('ref_axis',(0.951056516295154,0.,-0.309016994374947));
#17694=DIRECTION('center_axis',(0.,1.,0.));
#17695=DIRECTION('ref_axis',(1.,0.,0.));
#17696=DIRECTION('center_axis',(0.,1.,0.));
#17697=DIRECTION('ref_axis',(0.987688340595138,0.,-0.156434465040231));
#17698=DIRECTION('center_axis',(0.,1.,0.));
#17699=DIRECTION('ref_axis',(1.,0.,0.));
#17700=DIRECTION('center_axis',(0.,1.,0.));
#17701=DIRECTION('ref_axis',(1.,0.,0.));
#17702=DIRECTION('center_axis',(0.,1.,0.));
#17703=DIRECTION('ref_axis',(1.,0.,0.));
#17704=DIRECTION('center_axis',(0.,-1.,0.));
#17705=DIRECTION('ref_axis',(1.,0.,0.));
#17706=DIRECTION('center_axis',(0.,-1.,0.));
#17707=DIRECTION('ref_axis',(1.,0.,0.));
#17708=DIRECTION('',(0.,1.,0.));
#17709=DIRECTION('center_axis',(0.,1.,0.));
#17710=DIRECTION('ref_axis',(1.,0.,0.));
#17711=DIRECTION('center_axis',(0.,1.,0.));
#17712=DIRECTION('ref_axis',(1.,0.,0.));
#17713=DIRECTION('center_axis',(0.,1.,0.));
#17714=DIRECTION('ref_axis',(1.,0.,0.));
#17715=DIRECTION('center_axis',(0.,-1.,0.));
#17716=DIRECTION('ref_axis',(0.987688340595138,0.,0.156434465040231));
#17717=DIRECTION('center_axis',(0.,1.,0.));
#17718=DIRECTION('ref_axis',(1.,0.,0.));
#17719=DIRECTION('center_axis',(0.,-1.,0.));
#17720=DIRECTION('ref_axis',(1.,0.,0.));
#17721=DIRECTION('center_axis',(0.,1.,0.));
#17722=DIRECTION('ref_axis',(1.,0.,0.));
#17723=DIRECTION('center_axis',(0.,-1.,0.));
#17724=DIRECTION('ref_axis',(0.987688340595138,0.,-0.156434465040231));
#17725=DIRECTION('center_axis',(0.,1.,0.));
#17726=DIRECTION('ref_axis',(1.,0.,0.));
#17727=DIRECTION('center_axis',(0.,-1.,0.));
#17728=DIRECTION('ref_axis',(0.951056516295154,0.,-0.309016994374947));
#17729=DIRECTION('center_axis',(0.,1.,0.));
#17730=DIRECTION('ref_axis',(1.,0.,0.));
#17731=DIRECTION('center_axis',(0.,-1.,0.));
#17732=DIRECTION('ref_axis',(0.891006524188368,0.,-0.453990499739547));
#17733=DIRECTION('center_axis',(0.,1.,0.));
#17734=DIRECTION('ref_axis',(1.,0.,0.));
#17735=DIRECTION('center_axis',(0.,-1.,0.));
#17736=DIRECTION('ref_axis',(0.809016994374947,0.,-0.587785252292473));
#17737=DIRECTION('center_axis',(0.,1.,0.));
#17738=DIRECTION('ref_axis',(1.,0.,0.));
#17739=DIRECTION('center_axis',(0.,-1.,0.));
#17740=DIRECTION('ref_axis',(0.707106781186548,0.,-0.707106781186547));
#17741=DIRECTION('center_axis',(0.,1.,0.));
#17742=DIRECTION('ref_axis',(1.,0.,0.));
#17743=DIRECTION('center_axis',(0.,-1.,0.));
#17744=DIRECTION('ref_axis',(0.587785252292473,0.,-0.809016994374947));
#17745=DIRECTION('center_axis',(0.,1.,0.));
#17746=DIRECTION('ref_axis',(1.,0.,0.));
#17747=DIRECTION('center_axis',(0.,-1.,0.));
#17748=DIRECTION('ref_axis',(0.453990499739547,0.,-0.891006524188368));
#17749=DIRECTION('center_axis',(0.,1.,0.));
#17750=DIRECTION('ref_axis',(1.,0.,0.));
#17751=DIRECTION('center_axis',(0.,-1.,0.));
#17752=DIRECTION('ref_axis',(0.309016994374948,0.,-0.951056516295154));
#17753=DIRECTION('center_axis',(0.,1.,0.));
#17754=DIRECTION('ref_axis',(1.,0.,0.));
#17755=DIRECTION('center_axis',(0.,-1.,0.));
#17756=DIRECTION('ref_axis',(0.156434465040231,0.,-0.987688340595138));
#17757=DIRECTION('center_axis',(0.,1.,0.));
#17758=DIRECTION('ref_axis',(1.,0.,0.));
#17759=DIRECTION('center_axis',(0.,-1.,0.));
#17760=DIRECTION('ref_axis',(6.12323399573677E-17,0.,-1.));
#17761=DIRECTION('center_axis',(0.,1.,0.));
#17762=DIRECTION('ref_axis',(1.,0.,0.));
#17763=DIRECTION('center_axis',(0.,-1.,0.));
#17764=DIRECTION('ref_axis',(-0.156434465040231,0.,-0.987688340595138));
#17765=DIRECTION('center_axis',(0.,1.,0.));
#17766=DIRECTION('ref_axis',(1.,0.,0.));
#17767=DIRECTION('center_axis',(0.,-1.,0.));
#17768=DIRECTION('ref_axis',(-0.309016994374947,0.,-0.951056516295154));
#17769=DIRECTION('center_axis',(0.,1.,0.));
#17770=DIRECTION('ref_axis',(1.,0.,0.));
#17771=DIRECTION('center_axis',(0.,-1.,0.));
#17772=DIRECTION('ref_axis',(-0.453990499739547,0.,-0.891006524188368));
#17773=DIRECTION('center_axis',(0.,1.,0.));
#17774=DIRECTION('ref_axis',(1.,0.,0.));
#17775=DIRECTION('center_axis',(0.,-1.,0.));
#17776=DIRECTION('ref_axis',(-0.587785252292473,0.,-0.809016994374947));
#17777=DIRECTION('center_axis',(0.,1.,0.));
#17778=DIRECTION('ref_axis',(1.,0.,0.));
#17779=DIRECTION('center_axis',(0.,-1.,0.));
#17780=DIRECTION('ref_axis',(-0.707106781186547,0.,-0.707106781186548));
#17781=DIRECTION('center_axis',(0.,1.,0.));
#17782=DIRECTION('ref_axis',(1.,0.,0.));
#17783=DIRECTION('center_axis',(0.,-1.,0.));
#17784=DIRECTION('ref_axis',(-0.809016994374947,0.,-0.587785252292473));
#17785=DIRECTION('center_axis',(0.,1.,0.));
#17786=DIRECTION('ref_axis',(1.,0.,0.));
#17787=DIRECTION('center_axis',(0.,-1.,0.));
#17788=DIRECTION('ref_axis',(-0.891006524188368,0.,-0.453990499739547));
#17789=DIRECTION('center_axis',(0.,1.,0.));
#17790=DIRECTION('ref_axis',(1.,0.,0.));
#17791=DIRECTION('center_axis',(0.,-1.,0.));
#17792=DIRECTION('ref_axis',(-0.951056516295154,0.,-0.309016994374948));
#17793=DIRECTION('center_axis',(0.,1.,0.));
#17794=DIRECTION('ref_axis',(1.,0.,0.));
#17795=DIRECTION('center_axis',(0.,-1.,0.));
#17796=DIRECTION('ref_axis',(-0.987688340595138,0.,-0.156434465040231));
#17797=DIRECTION('center_axis',(0.,1.,0.));
#17798=DIRECTION('ref_axis',(1.,0.,0.));
#17799=DIRECTION('center_axis',(0.,-1.,0.));
#17800=DIRECTION('ref_axis',(-1.,0.,-1.22464679914735E-16));
#17801=DIRECTION('center_axis',(0.,1.,0.));
#17802=DIRECTION('ref_axis',(1.,0.,0.));
#17803=DIRECTION('center_axis',(0.,-1.,0.));
#17804=DIRECTION('ref_axis',(-0.987688340595138,0.,0.156434465040231));
#17805=DIRECTION('center_axis',(0.,1.,0.));
#17806=DIRECTION('ref_axis',(1.,0.,0.));
#17807=DIRECTION('center_axis',(0.,-1.,0.));
#17808=DIRECTION('ref_axis',(-0.951056516295154,0.,0.309016994374947));
#17809=DIRECTION('center_axis',(0.,1.,0.));
#17810=DIRECTION('ref_axis',(1.,0.,0.));
#17811=DIRECTION('center_axis',(0.,-1.,0.));
#17812=DIRECTION('ref_axis',(-0.891006524188368,0.,0.453990499739547));
#17813=DIRECTION('center_axis',(0.,1.,0.));
#17814=DIRECTION('ref_axis',(1.,0.,0.));
#17815=DIRECTION('center_axis',(0.,-1.,0.));
#17816=DIRECTION('ref_axis',(-0.809016994374947,0.,0.587785252292473));
#17817=DIRECTION('center_axis',(0.,1.,0.));
#17818=DIRECTION('ref_axis',(1.,0.,0.));
#17819=DIRECTION('center_axis',(0.,-1.,0.));
#17820=DIRECTION('ref_axis',(-0.707106781186548,0.,0.707106781186547));
#17821=DIRECTION('center_axis',(0.,1.,0.));
#17822=DIRECTION('ref_axis',(1.,0.,0.));
#17823=DIRECTION('center_axis',(0.,-1.,0.));
#17824=DIRECTION('ref_axis',(-0.587785252292473,0.,0.809016994374947));
#17825=DIRECTION('center_axis',(0.,1.,0.));
#17826=DIRECTION('ref_axis',(1.,0.,0.));
#17827=DIRECTION('center_axis',(0.,-1.,0.));
#17828=DIRECTION('ref_axis',(-0.453990499739547,0.,0.891006524188368));
#17829=DIRECTION('center_axis',(0.,1.,0.));
#17830=DIRECTION('ref_axis',(1.,0.,0.));
#17831=DIRECTION('center_axis',(0.,-1.,0.));
#17832=DIRECTION('ref_axis',(-0.309016994374948,0.,0.951056516295154));
#17833=DIRECTION('center_axis',(0.,1.,0.));
#17834=DIRECTION('ref_axis',(1.,0.,0.));
#17835=DIRECTION('center_axis',(0.,-1.,0.));
#17836=DIRECTION('ref_axis',(-0.156434465040231,0.,0.987688340595138));
#17837=DIRECTION('center_axis',(0.,1.,0.));
#17838=DIRECTION('ref_axis',(1.,0.,0.));
#17839=DIRECTION('center_axis',(0.,-1.,0.));
#17840=DIRECTION('ref_axis',(-1.83697019872103E-16,0.,1.));
#17841=DIRECTION('center_axis',(0.,1.,0.));
#17842=DIRECTION('ref_axis',(1.,0.,0.));
#17843=DIRECTION('center_axis',(0.,-1.,0.));
#17844=DIRECTION('ref_axis',(0.156434465040231,0.,0.987688340595138));
#17845=DIRECTION('center_axis',(0.,1.,0.));
#17846=DIRECTION('ref_axis',(1.,0.,0.));
#17847=DIRECTION('center_axis',(0.,-1.,0.));
#17848=DIRECTION('ref_axis',(0.309016994374947,0.,0.951056516295154));
#17849=DIRECTION('center_axis',(0.,1.,0.));
#17850=DIRECTION('ref_axis',(1.,0.,0.));
#17851=DIRECTION('center_axis',(0.,-1.,0.));
#17852=DIRECTION('ref_axis',(0.453990499739547,0.,0.891006524188368));
#17853=DIRECTION('center_axis',(0.,1.,0.));
#17854=DIRECTION('ref_axis',(1.,0.,0.));
#17855=DIRECTION('center_axis',(0.,-1.,0.));
#17856=DIRECTION('ref_axis',(0.587785252292473,0.,0.809016994374948));
#17857=DIRECTION('center_axis',(0.,1.,0.));
#17858=DIRECTION('ref_axis',(1.,0.,0.));
#17859=DIRECTION('center_axis',(0.,-1.,0.));
#17860=DIRECTION('ref_axis',(0.707106781186547,0.,0.707106781186548));
#17861=DIRECTION('center_axis',(0.,1.,0.));
#17862=DIRECTION('ref_axis',(1.,0.,0.));
#17863=DIRECTION('center_axis',(0.,-1.,0.));
#17864=DIRECTION('ref_axis',(0.809016994374947,0.,0.587785252292473));
#17865=DIRECTION('center_axis',(0.,1.,0.));
#17866=DIRECTION('ref_axis',(1.,0.,0.));
#17867=DIRECTION('center_axis',(0.,-1.,0.));
#17868=DIRECTION('ref_axis',(0.891006524188368,0.,0.453990499739547));
#17869=DIRECTION('center_axis',(0.,1.,0.));
#17870=DIRECTION('ref_axis',(1.,0.,0.));
#17871=DIRECTION('center_axis',(0.,-1.,0.));
#17872=DIRECTION('ref_axis',(0.951056516295154,0.,0.309016994374948));
#17873=DIRECTION('center_axis',(0.,1.,0.));
#17874=DIRECTION('ref_axis',(1.,0.,0.));
#17875=DIRECTION('center_axis',(0.,1.,0.));
#17876=DIRECTION('ref_axis',(1.,0.,0.));
#17877=DIRECTION('center_axis',(0.,1.,0.));
#17878=DIRECTION('ref_axis',(1.,0.,0.));
#17879=DIRECTION('',(0.,-1.,0.));
#17880=DIRECTION('center_axis',(0.,1.,0.));
#17881=DIRECTION('ref_axis',(1.,0.,0.));
#17882=DIRECTION('center_axis',(0.,1.,0.));
#17883=DIRECTION('ref_axis',(-0.987688340595137,0.,-0.156434465040233));
#17884=DIRECTION('',(0.,-1.,0.));
#17885=DIRECTION('',(0.,1.,0.));
#17886=DIRECTION('center_axis',(0.,1.,0.));
#17887=DIRECTION('ref_axis',(1.,0.,0.));
#17888=DIRECTION('',(0.,-1.,0.));
#17889=DIRECTION('center_axis',(0.,1.,0.));
#17890=DIRECTION('ref_axis',(-0.951056516295153,0.,-0.309016994374949));
#17891=DIRECTION('',(0.,1.,0.));
#17892=DIRECTION('center_axis',(0.,1.,0.));
#17893=DIRECTION('ref_axis',(1.,0.,0.));
#17894=DIRECTION('',(0.,-1.,0.));
#17895=DIRECTION('center_axis',(0.,1.,0.));
#17896=DIRECTION('ref_axis',(-0.891006524188368,0.,-0.453990499739547));
#17897=DIRECTION('',(0.,1.,0.));
#17898=DIRECTION('center_axis',(0.,1.,0.));
#17899=DIRECTION('ref_axis',(1.,0.,0.));
#17900=DIRECTION('',(0.,-1.,0.));
#17901=DIRECTION('center_axis',(0.,1.,0.));
#17902=DIRECTION('ref_axis',(-0.809016994374948,0.,-0.587785252292473));
#17903=DIRECTION('',(0.,1.,0.));
#17904=DIRECTION('center_axis',(0.,1.,0.));
#17905=DIRECTION('ref_axis',(1.,0.,0.));
#17906=DIRECTION('',(0.,-1.,0.));
#17907=DIRECTION('center_axis',(0.,1.,0.));
#17908=DIRECTION('ref_axis',(-0.707106781186547,0.,-0.707106781186548));
#17909=DIRECTION('',(0.,1.,0.));
#17910=DIRECTION('center_axis',(0.,1.,0.));
#17911=DIRECTION('ref_axis',(1.,0.,0.));
#17912=DIRECTION('',(0.,-1.,0.));
#17913=DIRECTION('center_axis',(0.,1.,0.));
#17914=DIRECTION('ref_axis',(-0.587785252292474,0.,-0.809016994374947));
#17915=DIRECTION('',(0.,1.,0.));
#17916=DIRECTION('center_axis',(0.,1.,0.));
#17917=DIRECTION('ref_axis',(1.,0.,0.));
#17918=DIRECTION('',(0.,-1.,0.));
#17919=DIRECTION('center_axis',(0.,1.,0.));
#17920=DIRECTION('ref_axis',(-0.453990499739547,0.,-0.891006524188368));
#17921=DIRECTION('',(0.,1.,0.));
#17922=DIRECTION('center_axis',(0.,1.,0.));
#17923=DIRECTION('ref_axis',(1.,0.,0.));
#17924=DIRECTION('',(0.,-1.,0.));
#17925=DIRECTION('center_axis',(0.,1.,0.));
#17926=DIRECTION('ref_axis',(-0.309016994374948,0.,-0.951056516295153));
#17927=DIRECTION('',(0.,1.,0.));
#17928=DIRECTION('center_axis',(0.,1.,0.));
#17929=DIRECTION('ref_axis',(1.,0.,0.));
#17930=DIRECTION('',(0.,-1.,0.));
#17931=DIRECTION('center_axis',(0.,1.,0.));
#17932=DIRECTION('ref_axis',(-0.156434465040232,0.,-0.987688340595138));
#17933=DIRECTION('',(0.,1.,0.));
#17934=DIRECTION('center_axis',(0.,1.,0.));
#17935=DIRECTION('ref_axis',(1.,0.,0.));
#17936=DIRECTION('',(0.,-1.,0.));
#17937=DIRECTION('center_axis',(0.,1.,0.));
#17938=DIRECTION('ref_axis',(3.06161699786838E-16,0.,-1.));
#17939=DIRECTION('',(0.,1.,0.));
#17940=DIRECTION('center_axis',(0.,1.,0.));
#17941=DIRECTION('ref_axis',(1.,0.,0.));
#17942=DIRECTION('',(0.,-1.,0.));
#17943=DIRECTION('center_axis',(0.,1.,0.));
#17944=DIRECTION('ref_axis',(0.156434465040233,0.,-0.987688340595138));
#17945=DIRECTION('',(0.,1.,0.));
#17946=DIRECTION('center_axis',(0.,1.,0.));
#17947=DIRECTION('ref_axis',(1.,0.,0.));
#17948=DIRECTION('',(0.,-1.,0.));
#17949=DIRECTION('center_axis',(0.,1.,0.));
#17950=DIRECTION('ref_axis',(0.309016994374946,0.,-0.951056516295154));
#17951=DIRECTION('',(0.,1.,0.));
#17952=DIRECTION('center_axis',(0.,1.,0.));
#17953=DIRECTION('ref_axis',(1.,0.,0.));
#17954=DIRECTION('',(0.,-1.,0.));
#17955=DIRECTION('center_axis',(0.,1.,0.));
#17956=DIRECTION('ref_axis',(0.453990499739547,0.,-0.891006524188368));
#17957=DIRECTION('',(0.,1.,0.));
#17958=DIRECTION('center_axis',(0.,1.,0.));
#17959=DIRECTION('ref_axis',(1.,0.,0.));
#17960=DIRECTION('',(0.,-1.,0.));
#17961=DIRECTION('center_axis',(0.,1.,0.));
#17962=DIRECTION('ref_axis',(0.587785252292473,0.,-0.809016994374947));
#17963=DIRECTION('',(0.,1.,0.));
#17964=DIRECTION('center_axis',(0.,1.,0.));
#17965=DIRECTION('ref_axis',(1.,0.,0.));
#17966=DIRECTION('',(0.,-1.,0.));
#17967=DIRECTION('center_axis',(0.,1.,0.));
#17968=DIRECTION('ref_axis',(0.707106781186548,0.,-0.707106781186547));
#17969=DIRECTION('',(0.,1.,0.));
#17970=DIRECTION('center_axis',(0.,1.,0.));
#17971=DIRECTION('ref_axis',(1.,0.,0.));
#17972=DIRECTION('',(0.,-1.,0.));
#17973=DIRECTION('center_axis',(0.,1.,0.));
#17974=DIRECTION('ref_axis',(0.809016994374946,0.,-0.587785252292475));
#17975=DIRECTION('',(0.,1.,0.));
#17976=DIRECTION('center_axis',(0.,1.,0.));
#17977=DIRECTION('ref_axis',(1.,0.,0.));
#17978=DIRECTION('',(0.,-1.,0.));
#17979=DIRECTION('center_axis',(0.,1.,0.));
#17980=DIRECTION('ref_axis',(0.891006524188368,0.,-0.453990499739547));
#17981=DIRECTION('',(0.,1.,0.));
#17982=DIRECTION('center_axis',(0.,1.,0.));
#17983=DIRECTION('ref_axis',(1.,0.,0.));
#17984=DIRECTION('',(0.,-1.,0.));
#17985=DIRECTION('center_axis',(0.,1.,0.));
#17986=DIRECTION('ref_axis',(0.951056516295154,0.,-0.309016994374946));
#17987=DIRECTION('',(0.,1.,0.));
#17988=DIRECTION('center_axis',(0.,1.,0.));
#17989=DIRECTION('ref_axis',(1.,0.,0.));
#17990=DIRECTION('',(0.,-1.,0.));
#17991=DIRECTION('center_axis',(0.,1.,0.));
#17992=DIRECTION('ref_axis',(0.987688340595138,0.,-0.156434465040232));
#17993=DIRECTION('',(0.,1.,0.));
#17994=DIRECTION('center_axis',(0.,1.,0.));
#17995=DIRECTION('ref_axis',(1.,0.,0.));
#17996=DIRECTION('',(0.,-1.,0.));
#17997=DIRECTION('center_axis',(0.,1.,0.));
#17998=DIRECTION('ref_axis',(1.,0.,2.44929359829471E-16));
#17999=DIRECTION('',(0.,1.,0.));
#18000=DIRECTION('center_axis',(0.,1.,0.));
#18001=DIRECTION('ref_axis',(1.,0.,0.));
#18002=DIRECTION('',(0.,-1.,0.));
#18003=DIRECTION('center_axis',(0.,1.,0.));
#18004=DIRECTION('ref_axis',(0.987688340595137,0.,0.156434465040232));
#18005=DIRECTION('',(0.,1.,0.));
#18006=DIRECTION('center_axis',(0.,1.,0.));
#18007=DIRECTION('ref_axis',(1.,0.,0.));
#18008=DIRECTION('',(0.,-1.,0.));
#18009=DIRECTION('center_axis',(0.,1.,0.));
#18010=DIRECTION('ref_axis',(0.951056516295154,0.,0.309016994374946));
#18011=DIRECTION('',(0.,1.,0.));
#18012=DIRECTION('center_axis',(0.,1.,0.));
#18013=DIRECTION('ref_axis',(1.,0.,0.));
#18014=DIRECTION('',(0.,-1.,0.));
#18015=DIRECTION('center_axis',(0.,1.,0.));
#18016=DIRECTION('ref_axis',(0.891006524188368,0.,0.453990499739547));
#18017=DIRECTION('',(0.,1.,0.));
#18018=DIRECTION('center_axis',(0.,1.,0.));
#18019=DIRECTION('ref_axis',(1.,0.,0.));
#18020=DIRECTION('',(0.,-1.,0.));
#18021=DIRECTION('center_axis',(0.,1.,0.));
#18022=DIRECTION('ref_axis',(0.809016994374947,0.,0.587785252292473));
#18023=DIRECTION('',(0.,1.,0.));
#18024=DIRECTION('center_axis',(0.,1.,0.));
#18025=DIRECTION('ref_axis',(1.,0.,0.));
#18026=DIRECTION('',(0.,-1.,0.));
#18027=DIRECTION('center_axis',(0.,1.,0.));
#18028=DIRECTION('ref_axis',(0.707106781186547,0.,0.707106781186548));
#18029=DIRECTION('',(0.,1.,0.));
#18030=DIRECTION('center_axis',(0.,1.,0.));
#18031=DIRECTION('ref_axis',(1.,0.,0.));
#18032=DIRECTION('',(0.,-1.,0.));
#18033=DIRECTION('center_axis',(0.,1.,0.));
#18034=DIRECTION('ref_axis',(0.587785252292475,0.,0.809016994374946));
#18035=DIRECTION('',(0.,1.,0.));
#18036=DIRECTION('center_axis',(0.,1.,0.));
#18037=DIRECTION('ref_axis',(1.,0.,0.));
#18038=DIRECTION('',(0.,-1.,0.));
#18039=DIRECTION('center_axis',(0.,1.,0.));
#18040=DIRECTION('ref_axis',(0.453990499739547,0.,0.891006524188368));
#18041=DIRECTION('',(0.,1.,0.));
#18042=DIRECTION('center_axis',(0.,1.,0.));
#18043=DIRECTION('ref_axis',(1.,0.,0.));
#18044=DIRECTION('',(0.,-1.,0.));
#18045=DIRECTION('center_axis',(0.,1.,0.));
#18046=DIRECTION('ref_axis',(0.309016994374946,0.,0.951056516295154));
#18047=DIRECTION('',(0.,1.,0.));
#18048=DIRECTION('center_axis',(0.,1.,0.));
#18049=DIRECTION('ref_axis',(1.,0.,0.));
#18050=DIRECTION('',(0.,-1.,0.));
#18051=DIRECTION('center_axis',(0.,1.,0.));
#18052=DIRECTION('ref_axis',(0.156434465040232,0.,0.987688340595138));
#18053=DIRECTION('',(0.,1.,0.));
#18054=DIRECTION('center_axis',(0.,1.,0.));
#18055=DIRECTION('ref_axis',(1.,0.,0.));
#18056=DIRECTION('',(0.,-1.,0.));
#18057=DIRECTION('center_axis',(0.,1.,0.));
#18058=DIRECTION('ref_axis',(-1.83697019872103E-16,0.,1.));
#18059=DIRECTION('',(0.,1.,0.));
#18060=DIRECTION('center_axis',(0.,1.,0.));
#18061=DIRECTION('ref_axis',(1.,0.,0.));
#18062=DIRECTION('',(0.,-1.,0.));
#18063=DIRECTION('center_axis',(0.,1.,0.));
#18064=DIRECTION('ref_axis',(-0.156434465040232,0.,0.987688340595138));
#18065=DIRECTION('',(0.,1.,0.));
#18066=DIRECTION('center_axis',(0.,1.,0.));
#18067=DIRECTION('ref_axis',(1.,0.,0.));
#18068=DIRECTION('',(0.,-1.,0.));
#18069=DIRECTION('center_axis',(0.,1.,0.));
#18070=DIRECTION('ref_axis',(-0.309016994374946,0.,0.951056516295154));
#18071=DIRECTION('',(0.,1.,0.));
#18072=DIRECTION('center_axis',(0.,1.,0.));
#18073=DIRECTION('ref_axis',(1.,0.,0.));
#18074=DIRECTION('',(0.,-1.,0.));
#18075=DIRECTION('center_axis',(0.,1.,0.));
#18076=DIRECTION('ref_axis',(-0.453990499739549,0.,0.891006524188367));
#18077=DIRECTION('',(0.,1.,0.));
#18078=DIRECTION('center_axis',(0.,1.,0.));
#18079=DIRECTION('ref_axis',(1.,0.,0.));
#18080=DIRECTION('',(0.,-1.,0.));
#18081=DIRECTION('center_axis',(0.,1.,0.));
#18082=DIRECTION('ref_axis',(-0.587785252292474,0.,0.809016994374947));
#18083=DIRECTION('',(0.,1.,0.));
#18084=DIRECTION('center_axis',(0.,1.,0.));
#18085=DIRECTION('ref_axis',(1.,0.,0.));
#18086=DIRECTION('',(0.,-1.,0.));
#18087=DIRECTION('center_axis',(0.,1.,0.));
#18088=DIRECTION('ref_axis',(-0.707106781186548,0.,0.707106781186547));
#18089=DIRECTION('',(0.,1.,0.));
#18090=DIRECTION('center_axis',(0.,1.,0.));
#18091=DIRECTION('ref_axis',(1.,0.,0.));
#18092=DIRECTION('',(0.,-1.,0.));
#18093=DIRECTION('center_axis',(0.,1.,0.));
#18094=DIRECTION('ref_axis',(-0.809016994374947,0.,0.587785252292474));
#18095=DIRECTION('',(0.,1.,0.));
#18096=DIRECTION('center_axis',(0.,1.,0.));
#18097=DIRECTION('ref_axis',(1.,0.,0.));
#18098=DIRECTION('',(0.,-1.,0.));
#18099=DIRECTION('center_axis',(0.,1.,0.));
#18100=DIRECTION('ref_axis',(-0.891006524188368,0.,0.453990499739547));
#18101=DIRECTION('',(0.,1.,0.));
#18102=DIRECTION('center_axis',(0.,1.,0.));
#18103=DIRECTION('ref_axis',(1.,0.,0.));
#18104=DIRECTION('',(0.,-1.,0.));
#18105=DIRECTION('center_axis',(0.,1.,0.));
#18106=DIRECTION('ref_axis',(-0.951056516295154,0.,0.309016994374948));
#18107=DIRECTION('',(0.,1.,0.));
#18108=DIRECTION('center_axis',(0.,1.,0.));
#18109=DIRECTION('ref_axis',(1.,0.,0.));
#18110=DIRECTION('',(0.,-1.,0.));
#18111=DIRECTION('center_axis',(0.,1.,0.));
#18112=DIRECTION('ref_axis',(-0.987688340595137,0.,0.156434465040233));
#18113=DIRECTION('',(0.,1.,0.));
#18114=DIRECTION('center_axis',(0.,1.,0.));
#18115=DIRECTION('ref_axis',(1.,0.,0.));
#18116=DIRECTION('',(0.,1.,0.));
#18117=DIRECTION('center_axis',(0.,1.,0.));
#18118=DIRECTION('ref_axis',(-1.,0.,-1.22464679914735E-16));
#18119=DIRECTION('',(0.,-1.,0.));
#18120=DIRECTION('center_axis',(0.,1.,0.));
#18121=DIRECTION('ref_axis',(1.,0.,0.));
#18122=DIRECTION('axis',(0.,0.,1.));
#18123=DIRECTION('refdir',(1.,0.,0.));
#18124=DIRECTION('center_axis',(0.,1.,0.));
#18125=DIRECTION('ref_axis',(0.,0.,1.));
#18126=DIRECTION('center_axis',(0.,-1.,0.));
#18127=DIRECTION('ref_axis',(1.,0.,0.));
#18128=DIRECTION('center_axis',(0.,-1.,0.));
#18129=DIRECTION('ref_axis',(1.,0.,0.));
#18130=DIRECTION('center_axis',(0.,-1.,0.));
#18131=DIRECTION('ref_axis',(1.,0.,0.));
#18132=DIRECTION('',(0.707106781186547,0.707106781186548,8.65956056235493E-17));
#18133=DIRECTION('center_axis',(0.,-1.,0.));
#18134=DIRECTION('ref_axis',(1.,0.,0.));
#18135=DIRECTION('center_axis',(0.,-1.,0.));
#18136=DIRECTION('ref_axis',(1.,0.,0.));
#18137=DIRECTION('',(0.,1.,0.));
#18138=DIRECTION('center_axis',(0.,1.,0.));
#18139=DIRECTION('ref_axis',(1.,0.,0.));
#18140=DIRECTION('center_axis',(0.,-1.,0.));
#18141=DIRECTION('ref_axis',(1.,0.,0.));
#18142=DIRECTION('',(-0.707106781186547,0.707106781186548,-8.65956056235493E-17));
#18143=DIRECTION('center_axis',(0.,-1.,0.));
#18144=DIRECTION('ref_axis',(0.,0.,-1.));
#18145=DIRECTION('center_axis',(0.,-1.,0.));
#18146=DIRECTION('ref_axis',(1.,0.,0.));
#18147=DIRECTION('center_axis',(0.,1.,0.));
#18148=DIRECTION('ref_axis',(1.,0.,0.));
#18149=DIRECTION('center_axis',(0.,1.,0.));
#18150=DIRECTION('ref_axis',(1.,0.,0.));
#18151=DIRECTION('',(-0.447213595499958,0.894427190999916,-5.47678698264203E-17));
#18152=DIRECTION('center_axis',(0.,-1.,0.));
#18153=DIRECTION('ref_axis',(1.,0.,0.));
#18154=DIRECTION('center_axis',(0.,1.,0.));
#18155=DIRECTION('ref_axis',(1.,0.,0.));
#18156=DIRECTION('',(0.,1.,0.));
#18157=DIRECTION('center_axis',(0.,1.,0.));
#18158=DIRECTION('ref_axis',(1.,0.,0.));
#18159=DIRECTION('center_axis',(0.,-1.,0.));
#18160=DIRECTION('ref_axis',(1.,0.,0.));
#18161=DIRECTION('',(-0.707106781186547,0.707106781186548,-8.65956056235493E-17));
#18162=DIRECTION('center_axis',(0.,-1.,0.));
#18163=DIRECTION('ref_axis',(0.,0.,-1.));
#18164=DIRECTION('center_axis',(0.866025403784439,0.,-0.5));
#18165=DIRECTION('ref_axis',(0.5,0.,0.866025403784439));
#18166=DIRECTION('',(-0.5,0.,-0.866025403784439));
#18167=DIRECTION('',(0.,-1.,0.));
#18168=DIRECTION('',(0.5,0.,0.866025403784439));
#18169=DIRECTION('',(0.,-1.,0.));
#18170=DIRECTION('center_axis',(1.60246890531964E-16,0.,-1.));
#18171=DIRECTION('ref_axis',(1.,0.,1.60246890531964E-16));
#18172=DIRECTION('',(-1.,0.,-1.60246890531964E-16));
#18173=DIRECTION('',(0.,-1.,0.));
#18174=DIRECTION('',(1.,0.,1.60246890531964E-16));
#18175=DIRECTION('center_axis',(-0.866025403784439,0.,-0.5));
#18176=DIRECTION('ref_axis',(0.5,0.,-0.866025403784439));
#18177=DIRECTION('',(-0.5,0.,0.866025403784439));
#18178=DIRECTION('',(0.,-1.,0.));
#18179=DIRECTION('',(0.5,0.,-0.866025403784439));
#18180=DIRECTION('center_axis',(-0.866025403784439,0.,0.5));
#18181=DIRECTION('ref_axis',(-0.5,0.,-0.866025403784439));
#18182=DIRECTION('',(0.5,0.,0.866025403784439));
#18183=DIRECTION('',(0.,-1.,0.));
#18184=DIRECTION('',(-0.5,0.,-0.866025403784439));
#18185=DIRECTION('center_axis',(-1.60246890531964E-16,0.,1.));
#18186=DIRECTION('ref_axis',(-1.,0.,-1.60246890531964E-16));
#18187=DIRECTION('',(1.,0.,1.60246890531964E-16));
#18188=DIRECTION('',(0.,-1.,0.));
#18189=DIRECTION('',(-1.,0.,-1.60246890531964E-16));
#18190=DIRECTION('center_axis',(0.866025403784439,0.,0.5));
#18191=DIRECTION('ref_axis',(-0.5,0.,0.866025403784439));
#18192=DIRECTION('',(0.5,0.,-0.866025403784439));
#18193=DIRECTION('',(-0.5,0.,0.866025403784439));
#18194=DIRECTION('center_axis',(0.,1.,0.));
#18195=DIRECTION('ref_axis',(1.,0.,0.));
#18196=DIRECTION('center_axis',(0.,-1.,0.));
#18197=DIRECTION('ref_axis',(0.,0.,-1.));
#18198=DIRECTION('',(0.,0.,1.));
#18199=DIRECTION('',(1.,0.,0.));
#18200=DIRECTION('',(0.,0.,1.));
#18201=DIRECTION('',(1.,0.,0.));
#18202=DIRECTION('',(0.,0.,1.));
#18203=DIRECTION('',(1.,0.,0.));
#18204=DIRECTION('',(0.,0.,1.));
#18205=DIRECTION('',(1.,0.,0.));
#18206=DIRECTION('',(0.,0.,1.));
#18207=DIRECTION('',(1.,0.,0.));
#18208=DIRECTION('',(0.,0.,1.));
#18209=DIRECTION('',(1.,0.,0.));
#18210=DIRECTION('',(0.,0.,1.));
#18211=DIRECTION('',(1.,0.,0.));
#18212=DIRECTION('',(0.,0.,1.));
#18213=DIRECTION('',(1.,0.,0.));
#18214=DIRECTION('',(0.,0.,1.));
#18215=DIRECTION('',(1.,0.,0.));
#18216=DIRECTION('',(0.,0.,1.));
#18217=DIRECTION('',(1.,0.,0.));
#18218=DIRECTION('',(0.,0.,1.));
#18219=DIRECTION('',(1.,0.,0.));
#18220=DIRECTION('',(0.,0.,1.));
#18221=DIRECTION('',(1.,0.,0.));
#18222=DIRECTION('',(0.,0.,1.));
#18223=DIRECTION('',(1.,0.,0.));
#18224=DIRECTION('',(0.,0.,1.));
#18225=DIRECTION('',(1.,0.,0.));
#18226=DIRECTION('',(0.,-1.,2.22044604925031E-16));
#18227=DIRECTION('',(1.,0.,0.));
#18228=DIRECTION('',(0.,-1.,2.22044604925031E-16));
#18229=DIRECTION('',(1.,0.,0.));
#18230=DIRECTION('',(0.,-1.,2.22044604925031E-16));
#18231=DIRECTION('',(1.,0.,0.));
#18232=DIRECTION('',(0.,-1.,2.22044604925031E-16));
#18233=DIRECTION('',(1.,0.,0.));
#18234=DIRECTION('',(0.,-1.,2.22044604925031E-16));
#18235=DIRECTION('',(1.,0.,0.));
#18236=DIRECTION('',(0.,-1.,2.22044604925031E-16));
#18237=DIRECTION('',(1.,0.,0.));
#18238=DIRECTION('',(0.,-1.,2.22044604925031E-16));
#18239=DIRECTION('',(1.,0.,0.));
#18240=DIRECTION('',(0.,-1.,2.22044604925031E-16));
#18241=DIRECTION('',(1.,0.,0.));
#18242=DIRECTION('',(0.,0.,1.));
#18243=DIRECTION('',(1.,0.,0.));
#18244=DIRECTION('',(0.,0.,1.));
#18245=DIRECTION('',(1.,0.,0.));
#18246=DIRECTION('',(0.,0.,1.));
#18247=DIRECTION('',(-1.,1.22464679914735E-16,0.));
#18248=DIRECTION('',(0.,0.,1.));
#18249=DIRECTION('',(-1.,1.22464679914735E-16,0.));
#18250=DIRECTION('',(0.,0.,1.));
#18251=DIRECTION('',(-1.,1.22464679914735E-16,0.));
#18252=DIRECTION('',(0.,0.,1.));
#18253=DIRECTION('',(-1.,1.22464679914735E-16,0.));
#18254=DIRECTION('',(0.,0.,1.));
#18255=DIRECTION('',(1.,0.,0.));
#18256=DIRECTION('',(0.,0.,1.));
#18257=DIRECTION('',(1.,0.,0.));
#18258=DIRECTION('',(0.,0.,1.));
#18259=DIRECTION('',(1.,0.,0.));
#18260=DIRECTION('',(0.,0.,1.));
#18261=DIRECTION('',(1.,0.,0.));
#18262=DIRECTION('',(0.,-1.,2.22044604925031E-16));
#18263=DIRECTION('',(1.,0.,0.));
#18264=DIRECTION('',(0.,-1.,2.22044604925031E-16));
#18265=DIRECTION('',(1.,0.,0.));
#18266=DIRECTION('',(0.,-1.,2.22044604925031E-16));
#18267=DIRECTION('',(1.,0.,0.));
#18268=DIRECTION('',(0.,-1.,2.22044604925031E-16));
#18269=DIRECTION('',(1.,0.,0.));
#18270=DIRECTION('',(0.,-1.,2.22044604925031E-16));
#18271=DIRECTION('',(1.,0.,0.));
#18272=DIRECTION('',(0.,-1.,2.22044604925031E-16));
#18273=DIRECTION('',(1.,0.,0.));
#18274=DIRECTION('',(0.,0.,1.));
#18275=DIRECTION('',(1.,0.,0.));
#18276=DIRECTION('',(0.,0.,1.));
#18277=DIRECTION('',(1.,0.,0.));
#18278=DIRECTION('',(0.,0.,1.));
#18279=DIRECTION('',(1.,0.,0.));
#18280=DIRECTION('',(0.,0.,1.));
#18281=DIRECTION('',(1.,0.,0.));
#18282=DIRECTION('',(0.,0.,1.));
#18283=DIRECTION('',(1.,0.,0.));
#18284=DIRECTION('',(0.,0.,1.));
#18285=DIRECTION('',(1.,0.,0.));
#18286=DIRECTION('',(0.,0.,1.));
#18287=DIRECTION('',(1.,0.,0.));
#18288=DIRECTION('',(0.,0.,1.));
#18289=DIRECTION('',(-1.,1.22464679914735E-16,0.));
#18290=DIRECTION('',(0.,0.,1.));
#18291=DIRECTION('',(1.,0.,0.));
#18292=DIRECTION('',(0.,0.,1.));
#18293=DIRECTION('',(1.,0.,0.));
#18294=DIRECTION('',(0.,0.,1.));
#18295=DIRECTION('',(1.,0.,0.));
#18296=DIRECTION('',(0.,0.,1.));
#18297=DIRECTION('',(1.,0.,0.));
#18298=DIRECTION('',(0.,0.,1.));
#18299=DIRECTION('',(1.,0.,0.));
#18300=DIRECTION('',(0.,0.,1.));
#18301=DIRECTION('',(1.,0.,0.));
#18302=DIRECTION('',(0.,0.,1.));
#18303=DIRECTION('',(1.,0.,0.));
#18304=DIRECTION('',(0.,0.,1.));
#18305=DIRECTION('',(-1.,1.22464679914735E-16,0.));
#18306=DIRECTION('axis',(0.,0.,1.));
#18307=DIRECTION('refdir',(1.,0.,0.));
#18308=DIRECTION('axis',(0.,0.,1.));
#18309=DIRECTION('refdir',(1.,0.,0.));
#18310=DIRECTION('center_axis',(1.,0.,0.));
#18311=DIRECTION('ref_axis',(0.,0.,-1.));
#18312=DIRECTION('center_axis',(1.,0.,0.));
#18313=DIRECTION('ref_axis',(0.,0.,-1.));
#18314=DIRECTION('',(-1.,0.,0.));
#18315=DIRECTION('center_axis',(1.,0.,0.));
#18316=DIRECTION('ref_axis',(0.,0.,-1.));
#18317=DIRECTION('center_axis',(1.,0.,0.));
#18318=DIRECTION('ref_axis',(0.,0.,-1.));
#18319=DIRECTION('center_axis',(1.,0.,0.));
#18320=DIRECTION('ref_axis',(0.,0.,-1.));
#18321=DIRECTION('center_axis',(1.,0.,0.));
#18322=DIRECTION('ref_axis',(0.,0.,-1.));
#18323=DIRECTION('center_axis',(1.,0.,0.));
#18324=DIRECTION('ref_axis',(0.,0.,-1.));
#18325=DIRECTION('center_axis',(1.,0.,0.));
#18326=DIRECTION('ref_axis',(0.,0.,-1.));
#18327=DIRECTION('center_axis',(1.,0.,0.));
#18328=DIRECTION('ref_axis',(0.,0.,-1.));
#18329=DIRECTION('center_axis',(-1.,0.,0.));
#18330=DIRECTION('ref_axis',(0.,0.,-1.));
#18331=DIRECTION('center_axis',(1.,0.,0.));
#18332=DIRECTION('ref_axis',(0.,0.,-1.));
#18333=DIRECTION('',(-1.,0.,0.));
#18334=DIRECTION('center_axis',(1.,0.,0.));
#18335=DIRECTION('ref_axis',(0.,0.,-1.));
#18336=DIRECTION('',(-1.,0.,0.));
#18337=DIRECTION('center_axis',(1.,0.,0.));
#18338=DIRECTION('ref_axis',(0.,0.,-1.));
#18339=DIRECTION('center_axis',(1.,0.,0.));
#18340=DIRECTION('ref_axis',(0.,0.,-1.));
#18341=DIRECTION('center_axis',(1.,0.,0.));
#18342=DIRECTION('ref_axis',(0.,0.,-1.));
#18343=DIRECTION('center_axis',(1.,0.,0.));
#18344=DIRECTION('ref_axis',(0.,0.,-1.));
#18345=DIRECTION('center_axis',(1.,0.,0.));
#18346=DIRECTION('ref_axis',(0.,0.,-1.));
#18347=DIRECTION('center_axis',(1.,0.,0.));
#18348=DIRECTION('ref_axis',(0.,0.,-1.));
#18349=DIRECTION('center_axis',(-1.,0.,0.));
#18350=DIRECTION('ref_axis',(0.,0.,-1.));
#18351=DIRECTION('center_axis',(1.,0.,0.));
#18352=DIRECTION('ref_axis',(0.,0.,-1.));
#18353=DIRECTION('',(-1.,0.,0.));
#18354=DIRECTION('center_axis',(1.,0.,0.));
#18355=DIRECTION('ref_axis',(0.,0.,-1.));
#18356=DIRECTION('',(-1.,0.,0.));
#18357=DIRECTION('center_axis',(1.,0.,0.));
#18358=DIRECTION('ref_axis',(0.,0.,-1.));
#18359=DIRECTION('center_axis',(1.,0.,0.));
#18360=DIRECTION('ref_axis',(0.,0.,-1.));
#18361=DIRECTION('center_axis',(-1.,0.,0.));
#18362=DIRECTION('ref_axis',(0.,0.,-1.));
#18363=DIRECTION('center_axis',(1.,0.,0.));
#18364=DIRECTION('ref_axis',(0.,0.,-1.));
#18365=DIRECTION('center_axis',(1.,0.,0.));
#18366=DIRECTION('ref_axis',(0.,0.,-1.));
#18367=DIRECTION('',(-1.,0.,0.));
#18368=DIRECTION('center_axis',(1.,0.,0.));
#18369=DIRECTION('ref_axis',(0.,0.,-1.));
#18370=DIRECTION('center_axis',(1.,0.,0.));
#18371=DIRECTION('ref_axis',(0.,0.,-1.));
#18372=DIRECTION('center_axis',(1.,0.,0.));
#18373=DIRECTION('ref_axis',(0.,0.,-1.));
#18374=DIRECTION('center_axis',(1.,0.,0.));
#18375=DIRECTION('ref_axis',(0.,0.,-1.));
#18376=DIRECTION('',(-1.,0.,0.));
#18377=DIRECTION('center_axis',(1.,0.,0.));
#18378=DIRECTION('ref_axis',(0.,0.,-1.));
#18379=DIRECTION('',(-1.,0.,0.));
#18380=DIRECTION('center_axis',(1.,0.,0.));
#18381=DIRECTION('ref_axis',(0.,0.,-1.));
#18382=DIRECTION('center_axis',(1.,0.,0.));
#18383=DIRECTION('ref_axis',(0.,0.,-1.));
#18384=DIRECTION('axis',(0.,0.,1.));
#18385=DIRECTION('refdir',(1.,0.,0.));
#18386=DIRECTION('center_axis',(0.,0.,1.));
#18387=DIRECTION('ref_axis',(1.,0.,0.));
#18388=DIRECTION('',(1.,0.,0.));
#18389=DIRECTION('center_axis',(0.,0.,1.));
#18390=DIRECTION('ref_axis',(1.,0.,0.));
#18391=DIRECTION('center_axis',(0.,0.,1.));
#18392=DIRECTION('ref_axis',(1.,0.,0.));
#18393=DIRECTION('center_axis',(0.,0.,1.));
#18394=DIRECTION('ref_axis',(1.,0.,0.));
#18395=DIRECTION('',(0.,0.,1.));
#18396=DIRECTION('center_axis',(0.,0.,1.));
#18397=DIRECTION('ref_axis',(1.,0.,0.));
#18398=DIRECTION('',(-1.,0.,0.));
#18399=DIRECTION('center_axis',(1.,0.,0.));
#18400=DIRECTION('ref_axis',(0.,0.,-1.));
#18401=DIRECTION('center_axis',(-1.,0.,0.));
#18402=DIRECTION('ref_axis',(0.,0.,-1.));
#18403=DIRECTION('',(-1.,0.,0.));
#18404=DIRECTION('',(-1.,0.,0.));
#18405=DIRECTION('center_axis',(-1.,0.,0.));
#18406=DIRECTION('ref_axis',(0.,0.,-1.));
#18407=DIRECTION('center_axis',(1.,0.,0.));
#18408=DIRECTION('ref_axis',(0.,0.,-1.));
#18409=DIRECTION('center_axis',(1.,0.,0.));
#18410=DIRECTION('ref_axis',(0.,0.,-1.));
#18411=DIRECTION('',(-1.,0.,0.));
#18412=DIRECTION('',(-1.,0.,0.));
#18413=DIRECTION('center_axis',(1.,0.,0.));
#18414=DIRECTION('ref_axis',(0.,0.,-1.));
#18415=DIRECTION('center_axis',(1.,0.,0.));
#18416=DIRECTION('ref_axis',(0.,0.,-1.));
#18417=DIRECTION('center_axis',(1.,0.,0.));
#18418=DIRECTION('ref_axis',(0.,0.,-1.));
#18419=DIRECTION('axis',(0.,0.,1.));
#18420=DIRECTION('refdir',(1.,0.,0.));
#18421=DIRECTION('center_axis',(0.866025403784439,0.,-0.5));
#18422=DIRECTION('ref_axis',(0.5,0.,0.866025403784439));
#18423=DIRECTION('',(0.5,0.,0.866025403784439));
#18424=DIRECTION('',(0.,-1.,0.));
#18425=DIRECTION('',(0.5,0.,0.866025403784439));
#18426=DIRECTION('',(0.,-1.,0.));
#18427=DIRECTION('center_axis',(1.20185167898973E-16,0.,-1.));
#18428=DIRECTION('ref_axis',(1.,0.,1.20185167898973E-16));
#18429=DIRECTION('',(1.,0.,1.20185167898973E-16));
#18430=DIRECTION('',(0.,-1.,0.));
#18431=DIRECTION('',(1.,0.,1.20185167898973E-16));
#18432=DIRECTION('center_axis',(-0.866025403784439,0.,-0.5));
#18433=DIRECTION('ref_axis',(0.5,0.,-0.866025403784439));
#18434=DIRECTION('',(0.5,0.,-0.866025403784439));
#18435=DIRECTION('',(0.,-1.,0.));
#18436=DIRECTION('',(0.5,0.,-0.866025403784439));
#18437=DIRECTION('center_axis',(-0.866025403784439,0.,0.5));
#18438=DIRECTION('ref_axis',(-0.5,0.,-0.866025403784439));
#18439=DIRECTION('',(-0.5,0.,-0.866025403784439));
#18440=DIRECTION('',(0.,-1.,0.));
#18441=DIRECTION('',(-0.5,0.,-0.866025403784439));
#18442=DIRECTION('center_axis',(-2.40370335797945E-16,0.,1.));
#18443=DIRECTION('ref_axis',(-1.,0.,-2.40370335797945E-16));
#18444=DIRECTION('',(-1.,0.,-2.40370335797945E-16));
#18445=DIRECTION('',(0.,-1.,0.));
#18446=DIRECTION('',(-1.,0.,-2.40370335797945E-16));
#18447=DIRECTION('center_axis',(0.866025403784439,0.,0.5));
#18448=DIRECTION('ref_axis',(-0.5,0.,0.866025403784439));
#18449=DIRECTION('',(-0.5,0.,0.866025403784439));
#18450=DIRECTION('',(-0.5,0.,0.866025403784439));
#18451=DIRECTION('center_axis',(0.,-1.,0.));
#18452=DIRECTION('ref_axis',(0.,0.,-1.));
#18453=DIRECTION('center_axis',(0.,1.,0.));
#18454=DIRECTION('ref_axis',(0.,0.,1.));
#18455=DIRECTION('center_axis',(0.,-1.,0.));
#18456=DIRECTION('ref_axis',(1.,0.,0.));
#18457=DIRECTION('center_axis',(0.,-1.,0.));
#18458=DIRECTION('ref_axis',(1.,0.,0.));
#18459=DIRECTION('center_axis',(0.,-1.,0.));
#18460=DIRECTION('ref_axis',(1.,0.,0.));
#18461=DIRECTION('',(0.707106781186548,0.707106781186547,8.65956056235494E-17));
#18462=DIRECTION('center_axis',(0.,-1.,0.));
#18463=DIRECTION('ref_axis',(1.,0.,0.));
#18464=DIRECTION('center_axis',(0.,1.,0.));
#18465=DIRECTION('ref_axis',(1.,0.,0.));
#18466=DIRECTION('',(0.,1.,0.));
#18467=DIRECTION('center_axis',(0.,1.,0.));
#18468=DIRECTION('ref_axis',(1.,0.,0.));
#18469=DIRECTION('center_axis',(0.,-1.,0.));
#18470=DIRECTION('ref_axis',(1.,0.,0.));
#18471=DIRECTION('',(-0.707106781186548,0.707106781186547,-8.65956056235494E-17));
#18472=DIRECTION('center_axis',(0.,-1.,0.));
#18473=DIRECTION('ref_axis',(0.,0.,-1.));
#18474=DIRECTION('',(0.,0.,1.));
#18475=DIRECTION('',(1.,0.,0.));
#18476=DIRECTION('',(0.,0.,1.));
#18477=DIRECTION('',(1.,0.,0.));
#18478=DIRECTION('',(0.,0.,1.));
#18479=DIRECTION('',(1.,0.,0.));
#18480=DIRECTION('',(0.,0.,1.));
#18481=DIRECTION('',(1.,0.,0.));
#18482=DIRECTION('',(0.,0.,1.));
#18483=DIRECTION('',(1.,0.,0.));
#18484=DIRECTION('',(0.,0.,1.));
#18485=DIRECTION('',(1.,0.,0.));
#18486=DIRECTION('',(0.,0.,1.));
#18487=DIRECTION('',(1.,0.,0.));
#18488=DIRECTION('',(0.,0.,1.));
#18489=DIRECTION('',(1.,0.,0.));
#18490=DIRECTION('',(0.,0.,1.));
#18491=DIRECTION('',(1.,0.,0.));
#18492=DIRECTION('',(0.,-1.,2.22044604925031E-16));
#18493=DIRECTION('',(1.,0.,0.));
#18494=DIRECTION('',(0.,-1.,2.22044604925031E-16));
#18495=DIRECTION('',(1.,0.,0.));
#18496=DIRECTION('',(0.,-1.,2.22044604925031E-16));
#18497=DIRECTION('',(1.,0.,0.));
#18498=DIRECTION('',(0.,-1.,2.22044604925031E-16));
#18499=DIRECTION('',(1.,0.,0.));
#18500=DIRECTION('',(0.,-1.,2.22044604925031E-16));
#18501=DIRECTION('',(1.,0.,0.));
#18502=DIRECTION('',(0.,-1.,2.22044604925031E-16));
#18503=DIRECTION('',(1.,0.,0.));
#18504=DIRECTION('',(0.,-1.,2.22044604925031E-16));
#18505=DIRECTION('',(1.,0.,0.));
#18506=DIRECTION('',(0.,-1.,2.22044604925031E-16));
#18507=DIRECTION('',(1.,0.,0.));
#18508=DIRECTION('',(0.,0.,1.));
#18509=DIRECTION('',(1.,0.,0.));
#18510=DIRECTION('',(0.,0.,1.));
#18511=DIRECTION('',(1.,0.,0.));
#18512=DIRECTION('',(0.,0.,1.));
#18513=DIRECTION('',(-1.,1.22464679914735E-16,0.));
#18514=DIRECTION('',(0.,0.,1.));
#18515=DIRECTION('',(-1.,1.22464679914735E-16,0.));
#18516=DIRECTION('',(0.,0.,1.));
#18517=DIRECTION('',(-1.,1.22464679914735E-16,0.));
#18518=DIRECTION('',(0.,0.,1.));
#18519=DIRECTION('',(-1.,1.22464679914735E-16,0.));
#18520=DIRECTION('',(0.,0.,1.));
#18521=DIRECTION('',(1.,0.,0.));
#18522=DIRECTION('',(0.,0.,1.));
#18523=DIRECTION('',(1.,0.,0.));
#18524=DIRECTION('',(0.,0.,1.));
#18525=DIRECTION('',(1.,0.,0.));
#18526=DIRECTION('',(0.,0.,1.));
#18527=DIRECTION('',(1.,0.,0.));
#18528=DIRECTION('',(0.,1.,2.22044604925031E-16));
#18529=DIRECTION('',(1.,0.,0.));
#18530=DIRECTION('',(0.,1.,2.22044604925031E-16));
#18531=DIRECTION('',(1.,0.,0.));
#18532=DIRECTION('',(0.,-1.,2.22044604925031E-16));
#18533=DIRECTION('',(1.,0.,0.));
#18534=DIRECTION('',(0.,0.,1.));
#18535=DIRECTION('',(1.,0.,0.));
#18536=DIRECTION('',(0.,0.,1.));
#18537=DIRECTION('',(1.,0.,0.));
#18538=DIRECTION('',(0.,-1.,2.22044604925031E-16));
#18539=DIRECTION('',(1.,0.,0.));
#18540=DIRECTION('',(0.,0.,1.));
#18541=DIRECTION('',(1.,0.,0.));
#18542=DIRECTION('',(0.,0.,1.));
#18543=DIRECTION('',(1.,0.,0.));
#18544=DIRECTION('',(0.,0.,1.));
#18545=DIRECTION('',(1.,0.,0.));
#18546=DIRECTION('',(0.,0.,1.));
#18547=DIRECTION('',(1.,0.,0.));
#18548=DIRECTION('',(0.,0.,1.));
#18549=DIRECTION('',(1.,0.,0.));
#18550=CARTESIAN_POINT('',(0.,0.,0.));
#18551=CARTESIAN_POINT('',(0.,0.,0.));
#18552=CARTESIAN_POINT('',(0.,0.,0.));
#18553=CARTESIAN_POINT('Origin',(3.,6.9,-1.1));
#18554=CARTESIAN_POINT('',(2.835,6.9,-1.1));
#18555=CARTESIAN_POINT('Origin',(3.,6.9,-1.1));
#18556=CARTESIAN_POINT('',(2.835,6.9,0.));
#18557=CARTESIAN_POINT('',(2.835,6.9,-1.1));
#18558=CARTESIAN_POINT('Origin',(3.,6.9,0.));
#18559=CARTESIAN_POINT('Origin',(3.,6.9,-1.1));
#18560=CARTESIAN_POINT('Origin',(3.,8.1,-1.1));
#18561=CARTESIAN_POINT('',(2.835,8.1,-1.1));
#18562=CARTESIAN_POINT('Origin',(3.,8.1,-1.1));
#18563=CARTESIAN_POINT('',(2.835,8.1,0.));
#18564=CARTESIAN_POINT('',(2.835,8.1,-1.1));
#18565=CARTESIAN_POINT('Origin',(3.,8.1,0.));
#18566=CARTESIAN_POINT('Origin',(3.,8.1,-1.1));
#18567=CARTESIAN_POINT('Origin',(22.25,9.5,-1.1));
#18568=CARTESIAN_POINT('',(22.085,9.5,-1.1));
#18569=CARTESIAN_POINT('Origin',(22.25,9.5,-1.1));
#18570=CARTESIAN_POINT('',(22.085,9.5,0.));
#18571=CARTESIAN_POINT('',(22.085,9.5,-1.1));
#18572=CARTESIAN_POINT('Origin',(22.25,9.5,0.));
#18573=CARTESIAN_POINT('Origin',(22.25,9.5,-1.1));
#18574=CARTESIAN_POINT('Origin',(22.25,12.5,-1.1));
#18575=CARTESIAN_POINT('',(22.085,12.5,-1.1));
#18576=CARTESIAN_POINT('Origin',(22.25,12.5,-1.1));
#18577=CARTESIAN_POINT('',(22.085,12.5,0.));
#18578=CARTESIAN_POINT('',(22.085,12.5,-1.1));
#18579=CARTESIAN_POINT('Origin',(22.25,12.5,0.));
#18580=CARTESIAN_POINT('Origin',(22.25,12.5,-1.1));
#18581=CARTESIAN_POINT('Origin',(2.75,9.5,-1.1));
#18582=CARTESIAN_POINT('',(2.585,9.5,-1.1));
#18583=CARTESIAN_POINT('Origin',(2.75,9.5,-1.1));
#18584=CARTESIAN_POINT('',(2.585,9.5,0.));
#18585=CARTESIAN_POINT('',(2.585,9.5,-1.1));
#18586=CARTESIAN_POINT('Origin',(2.75,9.5,0.));
#18587=CARTESIAN_POINT('Origin',(2.75,9.5,-1.1));
#18588=CARTESIAN_POINT('Origin',(2.75,12.5,-1.1));
#18589=CARTESIAN_POINT('',(2.585,12.5,-1.1));
#18590=CARTESIAN_POINT('Origin',(2.75,12.5,-1.1));
#18591=CARTESIAN_POINT('',(2.585,12.5,0.));
#18592=CARTESIAN_POINT('',(2.585,12.5,-1.1));
#18593=CARTESIAN_POINT('Origin',(2.75,12.5,0.));
#18594=CARTESIAN_POINT('Origin',(2.75,12.5,-1.1));
#18595=CARTESIAN_POINT('Origin',(2.8,-1.,-1.1));
#18596=CARTESIAN_POINT('',(2.635,-1.,-1.1));
#18597=CARTESIAN_POINT('Origin',(2.8,-1.,-1.1));
#18598=CARTESIAN_POINT('',(2.635,-1.,0.));
#18599=CARTESIAN_POINT('',(2.635,-1.,-1.1));
#18600=CARTESIAN_POINT('Origin',(2.8,-1.,0.));
#18601=CARTESIAN_POINT('Origin',(2.8,-1.,-1.1));
#18602=CARTESIAN_POINT('Origin',(-2.8,1.,-1.1));
#18603=CARTESIAN_POINT('',(-2.965,1.,-1.1));
#18604=CARTESIAN_POINT('Origin',(-2.8,1.,-1.1));
#18605=CARTESIAN_POINT('',(-2.965,1.,0.));
#18606=CARTESIAN_POINT('',(-2.965,1.,-1.1));
#18607=CARTESIAN_POINT('Origin',(-2.8,1.,0.));
#18608=CARTESIAN_POINT('Origin',(-2.8,1.,-1.1));
#18609=CARTESIAN_POINT('Origin',(-2.8,-1.,-1.1));
#18610=CARTESIAN_POINT('',(-2.965,-1.,-1.1));
#18611=CARTESIAN_POINT('Origin',(-2.8,-1.,-1.1));
#18612=CARTESIAN_POINT('',(-2.965,-1.,0.));
#18613=CARTESIAN_POINT('',(-2.965,-1.,-1.1));
#18614=CARTESIAN_POINT('Origin',(-2.8,-1.,0.));
#18615=CARTESIAN_POINT('Origin',(-2.8,-1.,-1.1));
#18616=CARTESIAN_POINT('Origin',(2.8,1.,-1.1));
#18617=CARTESIAN_POINT('',(2.635,1.,-1.1));
#18618=CARTESIAN_POINT('Origin',(2.8,1.,-1.1));
#18619=CARTESIAN_POINT('',(2.635,1.,0.));
#18620=CARTESIAN_POINT('',(2.635,1.,-1.1));
#18621=CARTESIAN_POINT('Origin',(2.8,1.,0.));
#18622=CARTESIAN_POINT('Origin',(2.8,1.,-1.1));
#18623=CARTESIAN_POINT('Origin',(18.,0.,-1.1));
#18624=CARTESIAN_POINT('',(17.835,-2.02066721859312E-17,-1.1));
#18625=CARTESIAN_POINT('Origin',(18.,0.,-1.1));
#18626=CARTESIAN_POINT('',(17.835,2.02066721859312E-17,0.));
#18627=CARTESIAN_POINT('',(17.835,-2.02066721859312E-17,-1.1));
#18628=CARTESIAN_POINT('Origin',(18.,0.,0.));
#18629=CARTESIAN_POINT('Origin',(18.,0.,-1.1));
#18630=CARTESIAN_POINT('Origin',(12.,0.,-1.1));
#18631=CARTESIAN_POINT('',(11.835,-2.02066721859312E-17,-1.1));
#18632=CARTESIAN_POINT('Origin',(12.,0.,-1.1));
#18633=CARTESIAN_POINT('',(11.835,2.02066721859312E-17,0.));
#18634=CARTESIAN_POINT('',(11.835,-2.02066721859312E-17,-1.1));
#18635=CARTESIAN_POINT('Origin',(12.,0.,0.));
#18636=CARTESIAN_POINT('Origin',(12.,0.,-1.1));
#18637=CARTESIAN_POINT('Origin',(6.,0.,-1.1));
#18638=CARTESIAN_POINT('',(5.835,-2.02066721859313E-17,-1.1));
#18639=CARTESIAN_POINT('Origin',(6.,0.,-1.1));
#18640=CARTESIAN_POINT('',(5.835,2.02066721859313E-17,0.));
#18641=CARTESIAN_POINT('',(5.835,-2.02066721859313E-17,-1.1));
#18642=CARTESIAN_POINT('Origin',(6.,0.,0.));
#18643=CARTESIAN_POINT('Origin',(6.,0.,-1.1));
#18644=CARTESIAN_POINT('Origin',(24.,0.,-1.1));
#18645=CARTESIAN_POINT('',(23.835,-2.02066721859312E-17,-1.1));
#18646=CARTESIAN_POINT('Origin',(24.,0.,-1.1));
#18647=CARTESIAN_POINT('',(23.835,2.02066721859312E-17,0.));
#18648=CARTESIAN_POINT('',(23.835,-2.02066721859312E-17,-1.1));
#18649=CARTESIAN_POINT('Origin',(24.,0.,0.));
#18650=CARTESIAN_POINT('Origin',(24.,0.,-1.1));
#18651=CARTESIAN_POINT('Origin',(26.,14.,-1.2));
#18652=CARTESIAN_POINT('',(26.,14.,-1.2));
#18653=CARTESIAN_POINT('',(-3.5,14.,-1.2));
#18654=CARTESIAN_POINT('',(26.,14.,-1.2));
#18655=CARTESIAN_POINT('',(-3.5,14.,0.));
#18656=CARTESIAN_POINT('',(-3.5,14.,-1.2));
#18657=CARTESIAN_POINT('',(26.,14.,0.));
#18658=CARTESIAN_POINT('',(26.,14.,0.));
#18659=CARTESIAN_POINT('',(26.,14.,-1.2));
#18660=CARTESIAN_POINT('Origin',(26.,-6.5,-1.2));
#18661=CARTESIAN_POINT('',(26.,-6.5,-1.2));
#18662=CARTESIAN_POINT('',(26.,-6.5,-1.2));
#18663=CARTESIAN_POINT('',(26.,-6.5,0.));
#18664=CARTESIAN_POINT('',(26.,-6.5,0.));
#18665=CARTESIAN_POINT('',(26.,-6.5,-1.2));
#18666=CARTESIAN_POINT('Origin',(-3.5,-6.5,-1.2));
#18667=CARTESIAN_POINT('',(-3.5,-6.5,-1.2));
#18668=CARTESIAN_POINT('',(-3.5,-6.5,-1.2));
#18669=CARTESIAN_POINT('',(-3.5,-6.5,0.));
#18670=CARTESIAN_POINT('',(-3.5,-6.5,0.));
#18671=CARTESIAN_POINT('',(-3.5,-6.5,-1.2));
#18672=CARTESIAN_POINT('Origin',(-3.5,14.,-1.2));
#18673=CARTESIAN_POINT('',(-3.5,14.,-1.2));
#18674=CARTESIAN_POINT('',(-3.5,14.,0.));
#18675=CARTESIAN_POINT('Origin',(11.25,3.75,0.));
#18676=CARTESIAN_POINT('Origin',(11.25,3.75,-1.2));
#18677=CARTESIAN_POINT('',(0.,0.,0.));
#18678=CARTESIAN_POINT('Origin',(-1.5,14.,-1.6));
#18679=CARTESIAN_POINT('',(-1.5,14.,-1.6));
#18680=CARTESIAN_POINT('',(-2.5,14.,-1.6));
#18681=CARTESIAN_POINT('',(-1.5,14.,-1.6));
#18682=CARTESIAN_POINT('',(-2.5,14.,-1.2));
#18683=CARTESIAN_POINT('',(-2.5,14.,-1.6));
#18684=CARTESIAN_POINT('',(-1.5,14.,-1.2));
#18685=CARTESIAN_POINT('',(-1.5,14.,-1.2));
#18686=CARTESIAN_POINT('',(-1.5,14.,-1.6));
#18687=CARTESIAN_POINT('Origin',(-1.5,-6.5,-1.6));
#18688=CARTESIAN_POINT('',(-1.5,-6.5,-1.6));
#18689=CARTESIAN_POINT('',(-1.5,-6.5,-1.6));
#18690=CARTESIAN_POINT('',(-1.5,-6.5,-1.2));
#18691=CARTESIAN_POINT('',(-1.5,-6.5,-1.2));
#18692=CARTESIAN_POINT('',(-1.5,-6.5,-1.6));
#18693=CARTESIAN_POINT('Origin',(-2.5,-6.5,-1.6));
#18694=CARTESIAN_POINT('',(-2.5,-6.5,-1.6));
#18695=CARTESIAN_POINT('',(-2.5,-6.5,-1.6));
#18696=CARTESIAN_POINT('',(-2.5,-6.5,-1.2));
#18697=CARTESIAN_POINT('',(-2.5,-6.5,-1.2));
#18698=CARTESIAN_POINT('',(-2.5,-6.5,-1.6));
#18699=CARTESIAN_POINT('Origin',(-2.5,14.,-1.6));
#18700=CARTESIAN_POINT('',(-2.5,14.,-1.6));
#18701=CARTESIAN_POINT('',(-2.5,14.,-1.2));
#18702=CARTESIAN_POINT('Origin',(-2.,3.75,-1.2));
#18703=CARTESIAN_POINT('Origin',(-2.,3.75,-1.6));
#18704=CARTESIAN_POINT('',(0.,0.,0.));
#18705=CARTESIAN_POINT('Origin',(25.,14.,-1.6));
#18706=CARTESIAN_POINT('',(25.,14.,-1.6));
#18707=CARTESIAN_POINT('',(24.,14.,-1.6));
#18708=CARTESIAN_POINT('',(25.,14.,-1.6));
#18709=CARTESIAN_POINT('',(24.,14.,-1.2));
#18710=CARTESIAN_POINT('',(24.,14.,-1.6));
#18711=CARTESIAN_POINT('',(25.,14.,-1.2));
#18712=CARTESIAN_POINT('',(25.,14.,-1.2));
#18713=CARTESIAN_POINT('',(25.,14.,-1.6));
#18714=CARTESIAN_POINT('Origin',(25.,-6.5,-1.6));
#18715=CARTESIAN_POINT('',(25.,-6.5,-1.6));
#18716=CARTESIAN_POINT('',(25.,-6.5,-1.6));
#18717=CARTESIAN_POINT('',(25.,-6.5,-1.2));
#18718=CARTESIAN_POINT('',(25.,-6.5,-1.2));
#18719=CARTESIAN_POINT('',(25.,-6.5,-1.6));
#18720=CARTESIAN_POINT('Origin',(24.,-6.5,-1.6));
#18721=CARTESIAN_POINT('',(24.,-6.5,-1.6));
#18722=CARTESIAN_POINT('',(24.,-6.5,-1.6));
#18723=CARTESIAN_POINT('',(24.,-6.5,-1.2));
#18724=CARTESIAN_POINT('',(24.,-6.5,-1.2));
#18725=CARTESIAN_POINT('',(24.,-6.5,-1.6));
#18726=CARTESIAN_POINT('Origin',(24.,14.,-1.6));
#18727=CARTESIAN_POINT('',(24.,14.,-1.6));
#18728=CARTESIAN_POINT('',(24.,14.,-1.2));
#18729=CARTESIAN_POINT('Origin',(24.5,3.75,-1.2));
#18730=CARTESIAN_POINT('Origin',(24.5,3.75,-1.6));
#18731=CARTESIAN_POINT('',(0.,0.,0.));
#18732=CARTESIAN_POINT('Origin',(-1.34350288425444,-1.9,5.65649711574556));
#18733=CARTESIAN_POINT('',(-1.50850288425444,-1.8,5.65649711574556));
#18734=CARTESIAN_POINT('Origin',(-1.34350288425444,-1.8,5.65649711574556));
#18735=CARTESIAN_POINT('',(-1.50850288425444,1.8,5.65649711574556));
#18736=CARTESIAN_POINT('',(-1.50850288425444,-1.9,5.65649711574556));
#18737=CARTESIAN_POINT('Origin',(-1.34350288425444,1.8,5.65649711574556));
#18738=CARTESIAN_POINT('Origin',(-1.34350288425444,-1.9,8.34350288425444));
#18739=CARTESIAN_POINT('',(-1.50850288425444,-1.8,8.34350288425444));
#18740=CARTESIAN_POINT('Origin',(-1.34350288425444,-1.8,8.34350288425444));
#18741=CARTESIAN_POINT('',(-1.50850288425444,1.8,8.34350288425444));
#18742=CARTESIAN_POINT('',(-1.50850288425444,-1.9,8.34350288425444));
#18743=CARTESIAN_POINT('Origin',(-1.34350288425444,1.8,8.34350288425444));
#18744=CARTESIAN_POINT('Origin',(1.34350288425444,-1.9,8.34350288425444));
#18745=CARTESIAN_POINT('',(1.17850288425444,-1.8,8.34350288425444));
#18746=CARTESIAN_POINT('Origin',(1.34350288425444,-1.8,8.34350288425444));
#18747=CARTESIAN_POINT('',(1.17850288425444,1.8,8.34350288425444));
#18748=CARTESIAN_POINT('',(1.17850288425444,-1.9,8.34350288425444));
#18749=CARTESIAN_POINT('Origin',(1.34350288425444,1.8,8.34350288425444));
#18750=CARTESIAN_POINT('Origin',(1.34350288425444,-1.9,5.65649711574556));
#18751=CARTESIAN_POINT('',(1.17850288425444,-1.8,5.65649711574556));
#18752=CARTESIAN_POINT('Origin',(1.34350288425444,-1.8,5.65649711574556));
#18753=CARTESIAN_POINT('',(1.17850288425444,1.8,5.65649711574556));
#18754=CARTESIAN_POINT('',(1.17850288425444,-1.9,5.65649711574556));
#18755=CARTESIAN_POINT('Origin',(1.34350288425444,1.8,5.65649711574556));
#18756=CARTESIAN_POINT('Origin',(0.,-1.9,7.));
#18757=CARTESIAN_POINT('',(-1.5,-1.8,7.));
#18758=CARTESIAN_POINT('Origin',(0.,-1.8,7.));
#18759=CARTESIAN_POINT('',(-1.5,1.8,7.));
#18760=CARTESIAN_POINT('',(-1.5,-1.9,7.));
#18761=CARTESIAN_POINT('Origin',(0.,1.8,7.));
#18762=CARTESIAN_POINT('Origin',(2.8,-1.,-0.1));
#18763=CARTESIAN_POINT('',(2.575,-1.,0.));
#18764=CARTESIAN_POINT('Origin',(2.8,-1.,0.));
#18765=CARTESIAN_POINT('',(2.575,-1.,0.8));
#18766=CARTESIAN_POINT('',(2.575,-1.,-0.1));
#18767=CARTESIAN_POINT('Origin',(2.8,-1.,0.8));
#18768=CARTESIAN_POINT('Origin',(-2.8,1.,-0.1));
#18769=CARTESIAN_POINT('',(-3.025,1.,0.));
#18770=CARTESIAN_POINT('Origin',(-2.8,1.,0.));
#18771=CARTESIAN_POINT('',(-3.025,1.,0.8));
#18772=CARTESIAN_POINT('',(-3.025,1.,-0.1));
#18773=CARTESIAN_POINT('Origin',(-2.8,1.,0.8));
#18774=CARTESIAN_POINT('Origin',(-2.8,-1.,-0.1));
#18775=CARTESIAN_POINT('',(-3.025,-1.,0.));
#18776=CARTESIAN_POINT('Origin',(-2.8,-1.,0.));
#18777=CARTESIAN_POINT('',(-3.025,-1.,0.8));
#18778=CARTESIAN_POINT('',(-3.025,-1.,-0.1));
#18779=CARTESIAN_POINT('Origin',(-2.8,-1.,0.8));
#18780=CARTESIAN_POINT('Origin',(2.8,1.,-0.1));
#18781=CARTESIAN_POINT('',(2.575,1.,0.));
#18782=CARTESIAN_POINT('Origin',(2.8,1.,0.));
#18783=CARTESIAN_POINT('',(2.575,1.,0.8));
#18784=CARTESIAN_POINT('',(2.575,1.,-0.1));
#18785=CARTESIAN_POINT('Origin',(2.8,1.,0.8));
#18786=CARTESIAN_POINT('Origin',(-3.4,-1.8,0.8));
#18787=CARTESIAN_POINT('',(2.2,-1.8,0.8));
#18788=CARTESIAN_POINT('',(2.2,1.8,0.8));
#18789=CARTESIAN_POINT('',(2.2,-1.8,0.8));
#18790=CARTESIAN_POINT('',(3.4,-1.8,0.8));
#18791=CARTESIAN_POINT('',(3.4,-1.8,0.8));
#18792=CARTESIAN_POINT('',(3.4,1.8,0.8));
#18793=CARTESIAN_POINT('',(3.4,-1.8,0.8));
#18794=CARTESIAN_POINT('',(3.4,1.8,0.8));
#18795=CARTESIAN_POINT('Origin',(-3.4,-1.8,0.8));
#18796=CARTESIAN_POINT('',(-2.2,1.8,0.8));
#18797=CARTESIAN_POINT('',(-2.2,-1.8,0.8));
#18798=CARTESIAN_POINT('',(-2.2,0.,0.8));
#18799=CARTESIAN_POINT('',(-3.4,1.8,0.8));
#18800=CARTESIAN_POINT('',(3.4,1.8,0.8));
#18801=CARTESIAN_POINT('',(-3.4,-1.8,0.8));
#18802=CARTESIAN_POINT('',(-3.4,-1.8,0.8));
#18803=CARTESIAN_POINT('',(3.4,-1.8,0.8));
#18804=CARTESIAN_POINT('Origin',(-3.4,-1.8,0.));
#18805=CARTESIAN_POINT('',(-3.4,-1.8,0.));
#18806=CARTESIAN_POINT('',(-3.4,-1.8,0.8));
#18807=CARTESIAN_POINT('',(-3.4,1.8,0.));
#18808=CARTESIAN_POINT('',(-3.4,1.8,0.8));
#18809=CARTESIAN_POINT('',(-3.4,-1.8,0.));
#18810=CARTESIAN_POINT('Origin',(3.4,-1.8,0.8));
#18811=CARTESIAN_POINT('',(3.4,-1.8,0.));
#18812=CARTESIAN_POINT('',(3.4,-1.8,0.));
#18813=CARTESIAN_POINT('',(3.4,1.8,0.));
#18814=CARTESIAN_POINT('',(3.4,-1.8,0.));
#18815=CARTESIAN_POINT('',(3.4,1.8,0.));
#18816=CARTESIAN_POINT('Origin',(-2.2,-1.8,0.));
#18817=CARTESIAN_POINT('',(2.2,-1.8,9.2));
#18818=CARTESIAN_POINT('',(2.2,-1.8,0.));
#18819=CARTESIAN_POINT('',(-2.2,-1.8,9.2));
#18820=CARTESIAN_POINT('',(-2.2,-1.8,9.2));
#18821=CARTESIAN_POINT('',(-2.2,-1.8,0.));
#18822=CARTESIAN_POINT('',(-3.4,-1.8,0.));
#18823=CARTESIAN_POINT('Origin',(2.2,-1.8,0.));
#18824=CARTESIAN_POINT('',(2.2,1.8,9.2));
#18825=CARTESIAN_POINT('',(2.2,1.8,0.));
#18826=CARTESIAN_POINT('',(2.2,-1.8,9.2));
#18827=CARTESIAN_POINT('Origin',(2.2,1.8,0.));
#18828=CARTESIAN_POINT('',(-2.2,1.8,9.2));
#18829=CARTESIAN_POINT('',(-2.2,1.8,0.));
#18830=CARTESIAN_POINT('',(2.2,1.8,9.2));
#18831=CARTESIAN_POINT('',(-3.4,1.8,0.));
#18832=CARTESIAN_POINT('Origin',(-2.2,1.8,0.));
#18833=CARTESIAN_POINT('',(-2.2,1.8,9.2));
#18834=CARTESIAN_POINT('Origin',(0.,0.,9.2));
#18835=CARTESIAN_POINT('Origin',(0.,0.,0.));
#18836=CARTESIAN_POINT('',(0.,0.,0.));
#18837=CARTESIAN_POINT('Origin',(0.,-0.45,7.));
#18838=CARTESIAN_POINT('',(-1.1,0.45,7.));
#18839=CARTESIAN_POINT('Origin',(0.,0.45,7.));
#18840=CARTESIAN_POINT('',(-1.1,-0.45,7.));
#18841=CARTESIAN_POINT('',(-1.1,-0.45,7.));
#18842=CARTESIAN_POINT('Origin',(0.,-0.45,7.));
#18843=CARTESIAN_POINT('Origin',(0.,-0.45,7.));
#18844=CARTESIAN_POINT('',(-1.49,0.45,7.));
#18845=CARTESIAN_POINT('Origin',(0.,0.45,7.));
#18846=CARTESIAN_POINT('',(-1.49,-0.45,7.));
#18847=CARTESIAN_POINT('',(-1.49,-0.45,7.));
#18848=CARTESIAN_POINT('Origin',(0.,-0.45,7.));
#18849=CARTESIAN_POINT('Origin',(0.,0.45,7.));
#18850=CARTESIAN_POINT('Origin',(0.,-0.45,7.));
#18851=CARTESIAN_POINT('',(0.,0.,0.));
#18852=CARTESIAN_POINT('Origin',(-1.34350288425444,-2.2,5.65649711574556));
#18853=CARTESIAN_POINT('',(-1.40634555589641,-2.1,5.4404512904656));
#18854=CARTESIAN_POINT('',(-1.40634555589641,-1.8,5.4404512904656));
#18855=CARTESIAN_POINT('',(-1.40634555589641,-2.2,5.4404512904656));
#18856=CARTESIAN_POINT('',(-1.5595487095344,-2.1,5.59365444410359));
#18857=CARTESIAN_POINT('Origin',(-1.34350288425444,-2.1,5.65649711574556));
#18858=CARTESIAN_POINT('',(-1.5595487095344,-1.8,5.59365444410359));
#18859=CARTESIAN_POINT('',(-1.5595487095344,-2.2,5.59365444410359));
#18860=CARTESIAN_POINT('Origin',(-1.34350288425444,-1.8,5.65649711574556));
#18861=CARTESIAN_POINT('Origin',(-1.34350288425444,-2.2,8.34350288425444));
#18862=CARTESIAN_POINT('',(-1.5595487095344,-2.1,8.40634555589641));
#18863=CARTESIAN_POINT('',(-1.5595487095344,-1.8,8.40634555589641));
#18864=CARTESIAN_POINT('',(-1.5595487095344,-2.2,8.40634555589641));
#18865=CARTESIAN_POINT('',(-1.40634555589641,-2.1,8.5595487095344));
#18866=CARTESIAN_POINT('Origin',(-1.34350288425444,-2.1,8.34350288425444));
#18867=CARTESIAN_POINT('',(-1.40634555589641,-1.8,8.5595487095344));
#18868=CARTESIAN_POINT('',(-1.40634555589641,-2.2,8.5595487095344));
#18869=CARTESIAN_POINT('Origin',(-1.34350288425444,-1.8,8.34350288425444));
#18870=CARTESIAN_POINT('Origin',(1.34350288425444,-2.2,8.34350288425444));
#18871=CARTESIAN_POINT('',(1.40634555589641,-2.1,8.5595487095344));
#18872=CARTESIAN_POINT('',(1.40634555589641,-1.8,8.5595487095344));
#18873=CARTESIAN_POINT('',(1.40634555589641,-2.2,8.5595487095344));
#18874=CARTESIAN_POINT('',(1.5595487095344,-2.1,8.40634555589641));
#18875=CARTESIAN_POINT('Origin',(1.34350288425444,-2.1,8.34350288425444));
#18876=CARTESIAN_POINT('',(1.5595487095344,-1.8,8.40634555589641));
#18877=CARTESIAN_POINT('',(1.5595487095344,-2.2,8.40634555589641));
#18878=CARTESIAN_POINT('Origin',(1.34350288425444,-1.8,8.34350288425444));
#18879=CARTESIAN_POINT('Origin',(1.34350288425444,-2.2,5.65649711574556));
#18880=CARTESIAN_POINT('',(1.5595487095344,-2.1,5.59365444410359));
#18881=CARTESIAN_POINT('',(1.5595487095344,-1.8,5.59365444410359));
#18882=CARTESIAN_POINT('',(1.5595487095344,-2.2,5.59365444410359));
#18883=CARTESIAN_POINT('',(1.40634555589641,-2.1,5.4404512904656));
#18884=CARTESIAN_POINT('Origin',(1.34350288425444,-2.1,5.65649711574556));
#18885=CARTESIAN_POINT('',(1.40634555589641,-1.8,5.4404512904656));
#18886=CARTESIAN_POINT('',(1.40634555589641,-2.2,5.4404512904656));
#18887=CARTESIAN_POINT('Origin',(1.34350288425444,-1.8,5.65649711574556));
#18888=CARTESIAN_POINT('Origin',(0.,-2.1,7.));
#18889=CARTESIAN_POINT('Origin',(0.,-2.1,7.));
#18890=CARTESIAN_POINT('Origin',(0.,-2.1,7.));
#18891=CARTESIAN_POINT('Origin',(0.,-2.1,7.));
#18892=CARTESIAN_POINT('Origin',(0.,-2.1,7.));
#18893=CARTESIAN_POINT('',(-1.1,-2.1,7.));
#18894=CARTESIAN_POINT('Origin',(0.,-2.1,7.));
#18895=CARTESIAN_POINT('Origin',(0.,-2.1,7.));
#18896=CARTESIAN_POINT('Origin',(0.,-1.8,7.));
#18897=CARTESIAN_POINT('Origin',(0.,-2.1,7.));
#18898=CARTESIAN_POINT('Origin',(0.,-1.8,7.));
#18899=CARTESIAN_POINT('Origin',(0.,-2.1,7.));
#18900=CARTESIAN_POINT('Origin',(0.,-1.8,7.));
#18901=CARTESIAN_POINT('Origin',(0.,-2.1,7.));
#18902=CARTESIAN_POINT('Origin',(0.,-1.8,7.));
#18903=CARTESIAN_POINT('Origin',(0.,-1.8,7.));
#18904=CARTESIAN_POINT('',(-1.49,-1.35,7.));
#18905=CARTESIAN_POINT('Origin',(0.,-1.35,7.));
#18906=CARTESIAN_POINT('',(-1.49,-1.8,7.));
#18907=CARTESIAN_POINT('',(-1.49,-1.8,7.));
#18908=CARTESIAN_POINT('Origin',(0.,-1.8,7.));
#18909=CARTESIAN_POINT('Origin',(0.,-1.35,7.));
#18910=CARTESIAN_POINT('',(-1.1,-1.35,7.));
#18911=CARTESIAN_POINT('Origin',(0.,-1.35,7.));
#18912=CARTESIAN_POINT('Origin',(0.,-2.1,7.));
#18913=CARTESIAN_POINT('',(-1.1,-2.1,7.));
#18914=CARTESIAN_POINT('Origin',(0.,-1.8,7.));
#18915=CARTESIAN_POINT('',(0.,0.,0.));
#18916=CARTESIAN_POINT('Origin',(-1.34350288425444,1.7,5.65649711574556));
#18917=CARTESIAN_POINT('',(-1.40634555589641,1.8,5.4404512904656));
#18918=CARTESIAN_POINT('',(-1.40634555589641,2.1,5.4404512904656));
#18919=CARTESIAN_POINT('',(-1.40634555589641,1.7,5.4404512904656));
#18920=CARTESIAN_POINT('',(-1.5595487095344,1.8,5.59365444410359));
#18921=CARTESIAN_POINT('Origin',(-1.34350288425444,1.8,5.65649711574556));
#18922=CARTESIAN_POINT('',(-1.5595487095344,2.1,5.59365444410359));
#18923=CARTESIAN_POINT('',(-1.5595487095344,1.7,5.59365444410359));
#18924=CARTESIAN_POINT('Origin',(-1.34350288425444,2.1,5.65649711574556));
#18925=CARTESIAN_POINT('Origin',(-1.34350288425444,1.7,8.34350288425444));
#18926=CARTESIAN_POINT('',(-1.5595487095344,1.8,8.40634555589641));
#18927=CARTESIAN_POINT('',(-1.5595487095344,2.1,8.40634555589641));
#18928=CARTESIAN_POINT('',(-1.5595487095344,1.7,8.40634555589641));
#18929=CARTESIAN_POINT('',(-1.40634555589641,1.8,8.5595487095344));
#18930=CARTESIAN_POINT('Origin',(-1.34350288425444,1.8,8.34350288425444));
#18931=CARTESIAN_POINT('',(-1.40634555589641,2.1,8.5595487095344));
#18932=CARTESIAN_POINT('',(-1.40634555589641,1.7,8.5595487095344));
#18933=CARTESIAN_POINT('Origin',(-1.34350288425444,2.1,8.34350288425444));
#18934=CARTESIAN_POINT('Origin',(1.34350288425444,1.7,8.34350288425444));
#18935=CARTESIAN_POINT('',(1.40634555589641,1.8,8.5595487095344));
#18936=CARTESIAN_POINT('',(1.40634555589641,2.1,8.5595487095344));
#18937=CARTESIAN_POINT('',(1.40634555589641,1.7,8.5595487095344));
#18938=CARTESIAN_POINT('',(1.5595487095344,1.8,8.40634555589641));
#18939=CARTESIAN_POINT('Origin',(1.34350288425444,1.8,8.34350288425444));
#18940=CARTESIAN_POINT('',(1.5595487095344,2.1,8.40634555589641));
#18941=CARTESIAN_POINT('',(1.5595487095344,1.7,8.40634555589641));
#18942=CARTESIAN_POINT('Origin',(1.34350288425444,2.1,8.34350288425444));
#18943=CARTESIAN_POINT('Origin',(1.34350288425444,1.7,5.65649711574556));
#18944=CARTESIAN_POINT('',(1.5595487095344,1.8,5.59365444410359));
#18945=CARTESIAN_POINT('',(1.5595487095344,2.1,5.59365444410359));
#18946=CARTESIAN_POINT('',(1.5595487095344,1.7,5.59365444410359));
#18947=CARTESIAN_POINT('',(1.40634555589641,1.8,5.4404512904656));
#18948=CARTESIAN_POINT('Origin',(1.34350288425444,1.8,5.65649711574556));
#18949=CARTESIAN_POINT('',(1.40634555589641,2.1,5.4404512904656));
#18950=CARTESIAN_POINT('',(1.40634555589641,1.7,5.4404512904656));
#18951=CARTESIAN_POINT('Origin',(1.34350288425444,2.1,5.65649711574556));
#18952=CARTESIAN_POINT('Origin',(0.,1.8,7.));
#18953=CARTESIAN_POINT('Origin',(0.,1.8,7.));
#18954=CARTESIAN_POINT('Origin',(0.,1.8,7.));
#18955=CARTESIAN_POINT('Origin',(0.,1.8,7.));
#18956=CARTESIAN_POINT('Origin',(0.,1.8,7.));
#18957=CARTESIAN_POINT('',(-1.49,1.8,7.));
#18958=CARTESIAN_POINT('Origin',(0.,1.8,7.));
#18959=CARTESIAN_POINT('Origin',(0.,1.8,7.));
#18960=CARTESIAN_POINT('Origin',(0.,2.1,7.));
#18961=CARTESIAN_POINT('Origin',(0.,1.8,7.));
#18962=CARTESIAN_POINT('Origin',(0.,2.1,7.));
#18963=CARTESIAN_POINT('Origin',(0.,1.8,7.));
#18964=CARTESIAN_POINT('Origin',(0.,2.1,7.));
#18965=CARTESIAN_POINT('Origin',(0.,1.8,7.));
#18966=CARTESIAN_POINT('Origin',(0.,2.1,7.));
#18967=CARTESIAN_POINT('Origin',(0.,1.35,7.));
#18968=CARTESIAN_POINT('',(-1.49,1.35,7.));
#18969=CARTESIAN_POINT('',(-1.49,1.35,7.));
#18970=CARTESIAN_POINT('Origin',(0.,1.35,7.));
#18971=CARTESIAN_POINT('Origin',(0.,1.35,7.));
#18972=CARTESIAN_POINT('',(-1.1,1.35,7.));
#18973=CARTESIAN_POINT('Origin',(0.,1.35,7.));
#18974=CARTESIAN_POINT('Origin',(0.,1.8,7.));
#18975=CARTESIAN_POINT('',(-1.1,2.1,7.));
#18976=CARTESIAN_POINT('Origin',(0.,2.1,7.));
#18977=CARTESIAN_POINT('',(-1.1,1.8,7.));
#18978=CARTESIAN_POINT('Origin',(0.,2.1,7.));
#18979=CARTESIAN_POINT('',(0.,0.,0.));
#18980=CARTESIAN_POINT('Origin',(2.75,9.5,0.6));
#18981=CARTESIAN_POINT('',(2.35,9.5,0.6));
#18982=CARTESIAN_POINT('Origin',(2.75,9.5,0.6));
#18983=CARTESIAN_POINT('',(2.35,9.5,6.));
#18984=CARTESIAN_POINT('',(2.35,9.5,0.6));
#18985=CARTESIAN_POINT('Origin',(2.75,9.5,6.));
#18986=CARTESIAN_POINT('Origin',(2.75,9.5,0.6));
#18987=CARTESIAN_POINT('',(2.525,9.5,0.6));
#18988=CARTESIAN_POINT('Origin',(2.75,9.5,0.6));
#18989=CARTESIAN_POINT('Origin',(2.75,12.5,0.6));
#18990=CARTESIAN_POINT('',(2.35,12.5,0.6));
#18991=CARTESIAN_POINT('Origin',(2.75,12.5,0.6));
#18992=CARTESIAN_POINT('',(2.35,12.5,6.));
#18993=CARTESIAN_POINT('',(2.35,12.5,0.6));
#18994=CARTESIAN_POINT('Origin',(2.75,12.5,6.));
#18995=CARTESIAN_POINT('Origin',(2.75,12.5,0.6));
#18996=CARTESIAN_POINT('',(2.525,12.5,0.6));
#18997=CARTESIAN_POINT('Origin',(2.75,12.5,0.6));
#18998=CARTESIAN_POINT('Origin',(2.75,9.5,-0.1));
#18999=CARTESIAN_POINT('',(2.525,9.5,0.));
#19000=CARTESIAN_POINT('Origin',(2.75,9.5,0.));
#19001=CARTESIAN_POINT('',(2.525,9.5,-0.1));
#19002=CARTESIAN_POINT('Origin',(2.75,12.5,-0.1));
#19003=CARTESIAN_POINT('',(2.525,12.5,0.));
#19004=CARTESIAN_POINT('Origin',(2.75,12.5,0.));
#19005=CARTESIAN_POINT('',(2.525,12.5,-0.1));
#19006=CARTESIAN_POINT('Origin',(1.9,11.,4.5));
#19007=CARTESIAN_POINT('',(2.,11.,5.3));
#19008=CARTESIAN_POINT('Origin',(2.,11.,4.5));
#19009=CARTESIAN_POINT('',(3.5,11.,5.3));
#19010=CARTESIAN_POINT('',(1.9,11.,5.3));
#19011=CARTESIAN_POINT('Origin',(3.5,11.,4.5));
#19012=CARTESIAN_POINT('Origin',(3.5,13.,0.));
#19013=CARTESIAN_POINT('',(3.5,13.,0.));
#19014=CARTESIAN_POINT('',(2.,13.,0.));
#19015=CARTESIAN_POINT('',(3.5,13.,0.));
#19016=CARTESIAN_POINT('',(2.,13.,6.));
#19017=CARTESIAN_POINT('',(2.,13.,0.));
#19018=CARTESIAN_POINT('',(3.5,13.,6.));
#19019=CARTESIAN_POINT('',(3.5,13.,6.));
#19020=CARTESIAN_POINT('',(3.5,13.,0.));
#19021=CARTESIAN_POINT('Origin',(3.5,9.,0.));
#19022=CARTESIAN_POINT('',(3.5,9.,0.));
#19023=CARTESIAN_POINT('',(3.5,9.,0.));
#19024=CARTESIAN_POINT('',(3.5,9.,6.));
#19025=CARTESIAN_POINT('',(3.5,9.,6.));
#19026=CARTESIAN_POINT('',(3.5,9.,0.));
#19027=CARTESIAN_POINT('Origin',(2.,9.,0.));
#19028=CARTESIAN_POINT('',(2.,9.,0.));
#19029=CARTESIAN_POINT('',(2.,9.,0.));
#19030=CARTESIAN_POINT('',(2.,9.,6.));
#19031=CARTESIAN_POINT('',(2.,9.,6.));
#19032=CARTESIAN_POINT('',(2.,9.,0.));
#19033=CARTESIAN_POINT('Origin',(2.,13.,0.));
#19034=CARTESIAN_POINT('',(2.,13.,0.));
#19035=CARTESIAN_POINT('',(2.,13.,6.));
#19036=CARTESIAN_POINT('Origin',(2.75,11.,6.));
#19037=CARTESIAN_POINT('Origin',(2.75,11.,0.));
#19038=CARTESIAN_POINT('',(0.,0.,0.));
#19039=CARTESIAN_POINT('Origin',(2.,11.,4.5));
#19040=CARTESIAN_POINT('',(3.5,11.,5.105));
#19041=CARTESIAN_POINT('Origin',(3.5,11.,4.5));
#19042=CARTESIAN_POINT('',(2.,11.,5.105));
#19043=CARTESIAN_POINT('',(2.,11.,5.105));
#19044=CARTESIAN_POINT('Origin',(2.,11.,4.5));
#19045=CARTESIAN_POINT('Origin',(2.,11.,4.5));
#19046=CARTESIAN_POINT('',(3.5,11.,5.3));
#19047=CARTESIAN_POINT('Origin',(3.5,11.,4.5));
#19048=CARTESIAN_POINT('',(2.,11.,5.3));
#19049=CARTESIAN_POINT('',(2.,11.,5.3));
#19050=CARTESIAN_POINT('Origin',(2.,11.,4.5));
#19051=CARTESIAN_POINT('Origin',(3.5,11.,4.5));
#19052=CARTESIAN_POINT('Origin',(2.,11.,4.5));
#19053=CARTESIAN_POINT('',(0.,0.,0.));
#19054=CARTESIAN_POINT('Origin',(22.25,9.5,0.6));
#19055=CARTESIAN_POINT('',(21.85,9.5,0.6));
#19056=CARTESIAN_POINT('Origin',(22.25,9.5,0.6));
#19057=CARTESIAN_POINT('',(21.85,9.5,6.));
#19058=CARTESIAN_POINT('',(21.85,9.5,0.6));
#19059=CARTESIAN_POINT('Origin',(22.25,9.5,6.));
#19060=CARTESIAN_POINT('Origin',(22.25,9.5,0.6));
#19061=CARTESIAN_POINT('',(22.025,9.5,0.6));
#19062=CARTESIAN_POINT('Origin',(22.25,9.5,0.6));
#19063=CARTESIAN_POINT('Origin',(22.25,12.5,0.6));
#19064=CARTESIAN_POINT('',(21.85,12.5,0.6));
#19065=CARTESIAN_POINT('Origin',(22.25,12.5,0.6));
#19066=CARTESIAN_POINT('',(21.85,12.5,6.));
#19067=CARTESIAN_POINT('',(21.85,12.5,0.6));
#19068=CARTESIAN_POINT('Origin',(22.25,12.5,6.));
#19069=CARTESIAN_POINT('Origin',(22.25,12.5,0.6));
#19070=CARTESIAN_POINT('',(22.025,12.5,0.6));
#19071=CARTESIAN_POINT('Origin',(22.25,12.5,0.6));
#19072=CARTESIAN_POINT('Origin',(22.25,9.5,-0.1));
#19073=CARTESIAN_POINT('',(22.025,9.5,0.));
#19074=CARTESIAN_POINT('Origin',(22.25,9.5,0.));
#19075=CARTESIAN_POINT('',(22.025,9.5,-0.1));
#19076=CARTESIAN_POINT('Origin',(22.25,12.5,-0.1));
#19077=CARTESIAN_POINT('',(22.025,12.5,0.));
#19078=CARTESIAN_POINT('Origin',(22.25,12.5,0.));
#19079=CARTESIAN_POINT('',(22.025,12.5,-0.1));
#19080=CARTESIAN_POINT('Origin',(21.4,11.,4.5));
#19081=CARTESIAN_POINT('',(21.5,11.,5.3));
#19082=CARTESIAN_POINT('Origin',(21.5,11.,4.5));
#19083=CARTESIAN_POINT('',(23.,11.,5.3));
#19084=CARTESIAN_POINT('',(21.4,11.,5.3));
#19085=CARTESIAN_POINT('Origin',(23.,11.,4.5));
#19086=CARTESIAN_POINT('Origin',(23.,13.,0.));
#19087=CARTESIAN_POINT('',(23.,13.,0.));
#19088=CARTESIAN_POINT('',(21.5,13.,0.));
#19089=CARTESIAN_POINT('',(23.,13.,0.));
#19090=CARTESIAN_POINT('',(21.5,13.,6.));
#19091=CARTESIAN_POINT('',(21.5,13.,0.));
#19092=CARTESIAN_POINT('',(23.,13.,6.));
#19093=CARTESIAN_POINT('',(23.,13.,6.));
#19094=CARTESIAN_POINT('',(23.,13.,0.));
#19095=CARTESIAN_POINT('Origin',(23.,9.,0.));
#19096=CARTESIAN_POINT('',(23.,9.,0.));
#19097=CARTESIAN_POINT('',(23.,9.,0.));
#19098=CARTESIAN_POINT('',(23.,9.,6.));
#19099=CARTESIAN_POINT('',(23.,9.,6.));
#19100=CARTESIAN_POINT('',(23.,9.,0.));
#19101=CARTESIAN_POINT('Origin',(21.5,9.,0.));
#19102=CARTESIAN_POINT('',(21.5,9.,0.));
#19103=CARTESIAN_POINT('',(21.5,9.,0.));
#19104=CARTESIAN_POINT('',(21.5,9.,6.));
#19105=CARTESIAN_POINT('',(21.5,9.,6.));
#19106=CARTESIAN_POINT('',(21.5,9.,0.));
#19107=CARTESIAN_POINT('Origin',(21.5,13.,0.));
#19108=CARTESIAN_POINT('',(21.5,13.,0.));
#19109=CARTESIAN_POINT('',(21.5,13.,6.));
#19110=CARTESIAN_POINT('Origin',(22.25,11.,6.));
#19111=CARTESIAN_POINT('Origin',(22.25,11.,0.));
#19112=CARTESIAN_POINT('',(0.,0.,0.));
#19113=CARTESIAN_POINT('Origin',(21.5,11.,4.5));
#19114=CARTESIAN_POINT('',(23.,11.,5.105));
#19115=CARTESIAN_POINT('Origin',(23.,11.,4.5));
#19116=CARTESIAN_POINT('',(21.5,11.,5.105));
#19117=CARTESIAN_POINT('',(21.5,11.,5.105));
#19118=CARTESIAN_POINT('Origin',(21.5,11.,4.5));
#19119=CARTESIAN_POINT('Origin',(21.5,11.,4.5));
#19120=CARTESIAN_POINT('',(23.,11.,5.3));
#19121=CARTESIAN_POINT('Origin',(23.,11.,4.5));
#19122=CARTESIAN_POINT('',(21.5,11.,5.3));
#19123=CARTESIAN_POINT('',(21.5,11.,5.3));
#19124=CARTESIAN_POINT('Origin',(21.5,11.,4.5));
#19125=CARTESIAN_POINT('Origin',(23.,11.,4.5));
#19126=CARTESIAN_POINT('Origin',(21.5,11.,4.5));
#19127=CARTESIAN_POINT('',(0.,0.,0.));
#19128=CARTESIAN_POINT('Origin',(2.,7.5,4.5));
#19129=CARTESIAN_POINT('',(9.5,7.5,4.81));
#19130=CARTESIAN_POINT('Origin',(9.5,7.5,4.5));
#19131=CARTESIAN_POINT('',(2.,7.5,4.81));
#19132=CARTESIAN_POINT('',(2.,7.5,4.81));
#19133=CARTESIAN_POINT('Origin',(2.,7.5,4.5));
#19134=CARTESIAN_POINT('Origin',(2.,7.5,4.5));
#19135=CARTESIAN_POINT('',(9.5,7.5,5.3));
#19136=CARTESIAN_POINT('Origin',(9.5,7.5,4.5));
#19137=CARTESIAN_POINT('',(2.,7.5,5.3));
#19138=CARTESIAN_POINT('',(2.,7.5,5.3));
#19139=CARTESIAN_POINT('Origin',(2.,7.5,4.5));
#19140=CARTESIAN_POINT('Origin',(9.5,7.5,4.5));
#19141=CARTESIAN_POINT('Origin',(2.,7.5,4.5));
#19142=CARTESIAN_POINT('',(0.,0.,0.));
#19143=CARTESIAN_POINT('Origin',(3.,8.1,0.6));
#19144=CARTESIAN_POINT('',(2.6,8.1,0.6));
#19145=CARTESIAN_POINT('',(2.6,8.09999999996984,3.97084973771869));
#19146=CARTESIAN_POINT('',(2.6,8.1,0.6));
#19147=CARTESIAN_POINT('',(3.,8.5,0.6));
#19148=CARTESIAN_POINT('Origin',(3.,8.1,0.6));
#19149=CARTESIAN_POINT('',(3.,8.5,4.5));
#19150=CARTESIAN_POINT('',(3.,8.5,0.6));
#19151=CARTESIAN_POINT('',(2.65358983848623,8.3,4.5));
#19152=CARTESIAN_POINT('Origin',(3.,8.1,4.5));
#19153=CARTESIAN_POINT('Ctrl Pts',(2.6,8.09999999993968,3.97084973771869));
#19154=CARTESIAN_POINT('Ctrl Pts',(2.59999999999099,8.15972702790978,4.0385738216565));
#19155=CARTESIAN_POINT('Ctrl Pts',(2.61364657269785,8.209952841357,4.11951904386589));
#19156=CARTESIAN_POINT('Ctrl Pts',(2.64131535047873,8.28146961928914,4.3010711770996));
#19157=CARTESIAN_POINT('Ctrl Pts',(2.65358983848622,8.3,4.40308295140713));
#19158=CARTESIAN_POINT('Ctrl Pts',(2.65358983848622,8.3,4.5));
#19159=CARTESIAN_POINT('Origin',(3.,6.9,0.6));
#19160=CARTESIAN_POINT('',(2.6,6.9,0.6));
#19161=CARTESIAN_POINT('',(2.6,6.90000000003016,3.97084973771869));
#19162=CARTESIAN_POINT('',(2.6,6.9,0.6));
#19163=CARTESIAN_POINT('',(3.,6.5,0.6));
#19164=CARTESIAN_POINT('Origin',(3.,6.9,0.6));
#19165=CARTESIAN_POINT('',(3.,6.5,4.5));
#19166=CARTESIAN_POINT('',(3.,6.5,0.6));
#19167=CARTESIAN_POINT('',(3.34641016151378,6.7,4.5));
#19168=CARTESIAN_POINT('Origin',(3.,6.9,4.5));
#19169=CARTESIAN_POINT('Ctrl Pts',(2.6,6.90000000006032,3.97084973771869));
#19170=CARTESIAN_POINT('Ctrl Pts',(2.60000000000072,6.90479404852274,3.96541379771789));
#19171=CARTESIAN_POINT('Ctrl Pts',(2.60008620085532,6.90964651743076,3.96006056814498));
#19172=CARTESIAN_POINT('Ctrl Pts',(2.60122740656895,6.94099338970816,3.92640010376094));
#19173=CARTESIAN_POINT('Ctrl Pts',(2.60512454705338,6.97203740815281,3.89755171629685));
#19174=CARTESIAN_POINT('Ctrl Pts',(2.6225443141011,7.03654018405112,3.8466291847403));
#19175=CARTESIAN_POINT('Ctrl Pts',(2.63623381415265,7.06993848403684,3.82453570130603));
#19176=CARTESIAN_POINT('Ctrl Pts',(2.66918291362779,7.12700799839143,3.79158660183088));
#19177=CARTESIAN_POINT('Ctrl Pts',(2.69015083258595,7.15550942144409,3.77743263176733));
#19178=CARTESIAN_POINT('Ctrl Pts',(2.74065869020899,7.20664909771142,3.75520298086526));
#19179=CARTESIAN_POINT('Ctrl Pts',(2.77021713882404,7.2292150185966,3.74700319058552));
#19180=CARTESIAN_POINT('Ctrl Pts',(2.82837641387987,7.26279329170595,3.73578055053196));
#19181=CARTESIAN_POINT('Ctrl Pts',(2.8615419983492,7.27697903270593,3.73165447370246));
#19182=CARTESIAN_POINT('Ctrl Pts',(2.93074503613534,7.29558509017111,3.72649645101547));
#19183=CARTESIAN_POINT('Ctrl Pts',(2.96677936981926,7.3,3.72540333075852));
#19184=CARTESIAN_POINT('Ctrl Pts',(3.03322063018074,7.3,3.72540333075852));
#19185=CARTESIAN_POINT('Ctrl Pts',(3.06925496386466,7.29558509017111,3.72649645101547));
#19186=CARTESIAN_POINT('Ctrl Pts',(3.1384580016508,7.27697903270593,3.73165447370246));
#19187=CARTESIAN_POINT('Ctrl Pts',(3.17162358612013,7.26279329170596,3.73578055053196));
#19188=CARTESIAN_POINT('Ctrl Pts',(3.22978286117596,7.2292150185966,3.74700319058552));
#19189=CARTESIAN_POINT('Ctrl Pts',(3.25934130979101,7.20664909771142,3.75520298086526));
#19190=CARTESIAN_POINT('Ctrl Pts',(3.30984916741405,7.15550942144409,3.77743263176733));
#19191=CARTESIAN_POINT('Ctrl Pts',(3.33081708637221,7.12700799839143,3.79158660183088));
#19192=CARTESIAN_POINT('Ctrl Pts',(3.36376618584735,7.06993848403684,3.82453570130603));
#19193=CARTESIAN_POINT('Ctrl Pts',(3.3774556858989,7.03654018405112,3.8466291847403));
#19194=CARTESIAN_POINT('Ctrl Pts',(3.39487545294662,6.97203740815281,3.89755171629685));
#19195=CARTESIAN_POINT('Ctrl Pts',(3.39877259343105,6.94099338970816,3.92640010376094));
#19196=CARTESIAN_POINT('Ctrl Pts',(3.40213904264749,6.84852307313348,4.02569529883171));
#19197=CARTESIAN_POINT('Ctrl Pts',(3.38742101269684,6.79280659630953,4.11251394926614));
#19198=CARTESIAN_POINT('Ctrl Pts',(3.35868464952127,6.71853038071086,4.3010711770996));
#19199=CARTESIAN_POINT('Ctrl Pts',(3.34641016151378,6.7,4.40308295140713));
#19200=CARTESIAN_POINT('Ctrl Pts',(3.34641016151378,6.7,4.5));
#19201=CARTESIAN_POINT('Origin',(3.,6.9,0.6));
#19202=CARTESIAN_POINT('',(2.65358983848622,6.7,4.5));
#19203=CARTESIAN_POINT('Ctrl Pts',(2.65358983848622,6.7,4.5));
#19204=CARTESIAN_POINT('Ctrl Pts',(2.65358983848622,6.7,4.40308295140713));
#19205=CARTESIAN_POINT('Ctrl Pts',(2.64131535047873,6.71853038071086,4.3010711770996));
#19206=CARTESIAN_POINT('Ctrl Pts',(2.61364657269785,6.790047158643,4.11951904386589));
#19207=CARTESIAN_POINT('Ctrl Pts',(2.59999999999099,6.84027297209022,4.0385738216565));
#19208=CARTESIAN_POINT('Ctrl Pts',(2.6,6.90000000006032,3.97084973771869));
#19209=CARTESIAN_POINT('Origin',(3.,6.9,4.5));
#19210=CARTESIAN_POINT('',(3.,6.5,0.6));
#19211=CARTESIAN_POINT('Origin',(3.,6.9,0.6));
#19212=CARTESIAN_POINT('Origin',(3.,6.9,0.6));
#19213=CARTESIAN_POINT('',(2.775,6.9,0.6));
#19214=CARTESIAN_POINT('Origin',(3.,6.9,0.6));
#19215=CARTESIAN_POINT('Origin',(3.,8.1,0.6));
#19216=CARTESIAN_POINT('',(3.34641016151377,8.3,4.5));
#19217=CARTESIAN_POINT('Ctrl Pts',(3.34641016151378,8.3,4.5));
#19218=CARTESIAN_POINT('Ctrl Pts',(3.34641016151378,8.3,4.40308295140713));
#19219=CARTESIAN_POINT('Ctrl Pts',(3.35868464952127,8.28146961928914,4.3010711770996));
#19220=CARTESIAN_POINT('Ctrl Pts',(3.38742101269684,8.20719340369047,4.11251394926615));
#19221=CARTESIAN_POINT('Ctrl Pts',(3.40213904264749,8.15147692686652,4.02569529883171));
#19222=CARTESIAN_POINT('Ctrl Pts',(3.39877259343105,8.05900661029184,3.92640010376094));
#19223=CARTESIAN_POINT('Ctrl Pts',(3.39487545294662,8.02796259184719,3.89755171629685));
#19224=CARTESIAN_POINT('Ctrl Pts',(3.3774556858989,7.96345981594888,3.8466291847403));
#19225=CARTESIAN_POINT('Ctrl Pts',(3.36376618584735,7.93006151596316,3.82453570130603));
#19226=CARTESIAN_POINT('Ctrl Pts',(3.33081708637221,7.87299200160857,3.79158660183088));
#19227=CARTESIAN_POINT('Ctrl Pts',(3.30984916741405,7.84449057855591,3.77743263176733));
#19228=CARTESIAN_POINT('Ctrl Pts',(3.25934130979101,7.79335090228858,3.75520298086526));
#19229=CARTESIAN_POINT('Ctrl Pts',(3.22978286117596,7.7707849814034,3.74700319058552));
#19230=CARTESIAN_POINT('Ctrl Pts',(3.17162358612013,7.73720670829404,3.73578055053196));
#19231=CARTESIAN_POINT('Ctrl Pts',(3.1384580016508,7.72302096729407,3.73165447370246));
#19232=CARTESIAN_POINT('Ctrl Pts',(3.06925496386466,7.70441490982889,3.72649645101547));
#19233=CARTESIAN_POINT('Ctrl Pts',(3.03322063018074,7.7,3.72540333075852));
#19234=CARTESIAN_POINT('Ctrl Pts',(2.96677936981926,7.7,3.72540333075852));
#19235=CARTESIAN_POINT('Ctrl Pts',(2.93074503613534,7.70441490982889,3.72649645101547));
#19236=CARTESIAN_POINT('Ctrl Pts',(2.8615419983492,7.72302096729407,3.73165447370246));
#19237=CARTESIAN_POINT('Ctrl Pts',(2.82837641387987,7.73720670829404,3.73578055053196));
#19238=CARTESIAN_POINT('Ctrl Pts',(2.77021713882404,7.7707849814034,3.74700319058552));
#19239=CARTESIAN_POINT('Ctrl Pts',(2.74065869020899,7.79335090228858,3.75520298086526));
#19240=CARTESIAN_POINT('Ctrl Pts',(2.69015083258595,7.84449057855591,3.77743263176733));
#19241=CARTESIAN_POINT('Ctrl Pts',(2.66918291362779,7.87299200160857,3.79158660183088));
#19242=CARTESIAN_POINT('Ctrl Pts',(2.63623381415265,7.93006151596316,3.82453570130603));
#19243=CARTESIAN_POINT('Ctrl Pts',(2.6225443141011,7.96345981594888,3.8466291847403));
#19244=CARTESIAN_POINT('Ctrl Pts',(2.60512454705338,8.02796259184719,3.89755171629685));
#19245=CARTESIAN_POINT('Ctrl Pts',(2.60122740656895,8.05900661029184,3.92640010376094));
#19246=CARTESIAN_POINT('Ctrl Pts',(2.60008620085532,8.09035348256924,3.96006056814498));
#19247=CARTESIAN_POINT('Ctrl Pts',(2.60000000000072,8.09520595147726,3.96541379771789));
#19248=CARTESIAN_POINT('Ctrl Pts',(2.6,8.09999999993968,3.97084973771869));
#19249=CARTESIAN_POINT('Origin',(3.,8.1,4.5));
#19250=CARTESIAN_POINT('',(3.,8.5,0.6));
#19251=CARTESIAN_POINT('Origin',(3.,8.1,0.6));
#19252=CARTESIAN_POINT('Origin',(3.,8.1,0.6));
#19253=CARTESIAN_POINT('',(2.775,8.1,0.6));
#19254=CARTESIAN_POINT('Origin',(3.,8.1,0.6));
#19255=CARTESIAN_POINT('Origin',(3.,7.5,4.5));
#19256=CARTESIAN_POINT('',(2.,6.7,4.5));
#19257=CARTESIAN_POINT('',(1.9,6.7,4.5));
#19258=CARTESIAN_POINT('',(2.,6.5,4.5));
#19259=CARTESIAN_POINT('',(2.,8.5,4.5));
#19260=CARTESIAN_POINT('',(2.,6.5,4.5));
#19261=CARTESIAN_POINT('Origin',(3.,7.5,4.5));
#19262=CARTESIAN_POINT('',(4.,8.3,4.5));
#19263=CARTESIAN_POINT('',(1.9,8.3,4.5));
#19264=CARTESIAN_POINT('',(4.,8.5,4.5));
#19265=CARTESIAN_POINT('',(4.,6.5,4.5));
#19266=CARTESIAN_POINT('',(4.,8.5,4.5));
#19267=CARTESIAN_POINT('Origin',(3.,7.5,4.5));
#19268=CARTESIAN_POINT('',(2.,8.5,4.5));
#19269=CARTESIAN_POINT('',(4.,8.5,4.5));
#19270=CARTESIAN_POINT('',(2.,8.3,4.5));
#19271=CARTESIAN_POINT('',(2.,8.5,4.5));
#19272=CARTESIAN_POINT('',(1.9,8.3,4.5));
#19273=CARTESIAN_POINT('Origin',(3.,6.9,-0.1));
#19274=CARTESIAN_POINT('',(2.775,6.9,0.));
#19275=CARTESIAN_POINT('Origin',(3.,6.9,0.));
#19276=CARTESIAN_POINT('',(2.775,6.9,-0.1));
#19277=CARTESIAN_POINT('Origin',(3.,8.1,-0.1));
#19278=CARTESIAN_POINT('',(2.775,8.1,0.));
#19279=CARTESIAN_POINT('Origin',(3.,8.1,0.));
#19280=CARTESIAN_POINT('',(2.775,8.1,-0.1));
#19281=CARTESIAN_POINT('Origin',(1.9,7.5,4.5));
#19282=CARTESIAN_POINT('',(4.,6.7,4.5));
#19283=CARTESIAN_POINT('',(1.9,6.7,4.5));
#19284=CARTESIAN_POINT('Origin',(4.,7.5,4.5));
#19285=CARTESIAN_POINT('Origin',(2.,7.5,4.5));
#19286=CARTESIAN_POINT('Origin',(4.,6.5,0.));
#19287=CARTESIAN_POINT('',(4.,6.5,4.5));
#19288=CARTESIAN_POINT('',(4.,6.5,4.5));
#19289=CARTESIAN_POINT('',(4.,6.5,0.));
#19290=CARTESIAN_POINT('',(4.,6.5,0.));
#19291=CARTESIAN_POINT('',(4.,8.5,0.));
#19292=CARTESIAN_POINT('',(4.,6.5,0.));
#19293=CARTESIAN_POINT('',(4.,8.5,0.));
#19294=CARTESIAN_POINT('Origin',(3.,7.5,4.5));
#19295=CARTESIAN_POINT('',(2.,6.5,4.5));
#19296=CARTESIAN_POINT('Origin',(4.,8.5,0.));
#19297=CARTESIAN_POINT('',(2.,8.5,0.));
#19298=CARTESIAN_POINT('',(4.,8.5,0.));
#19299=CARTESIAN_POINT('',(2.,8.5,0.));
#19300=CARTESIAN_POINT('Origin',(2.,6.5,0.));
#19301=CARTESIAN_POINT('',(2.,6.5,0.));
#19302=CARTESIAN_POINT('',(2.,6.5,0.));
#19303=CARTESIAN_POINT('',(2.,6.5,0.));
#19304=CARTESIAN_POINT('Origin',(2.,8.5,0.));
#19305=CARTESIAN_POINT('',(2.,8.5,0.));
#19306=CARTESIAN_POINT('Origin',(3.,7.5,0.));
#19307=CARTESIAN_POINT('',(0.,0.,0.));
#19308=CARTESIAN_POINT('Origin',(14.,0.,0.97));
#19309=CARTESIAN_POINT('',(13.625,-4.59242549680257E-17,0.97));
#19310=CARTESIAN_POINT('Origin',(14.,0.,0.97));
#19311=CARTESIAN_POINT('',(13.625,4.59242549680257E-17,1.5));
#19312=CARTESIAN_POINT('',(13.625,-4.59242549680257E-17,0.97));
#19313=CARTESIAN_POINT('Origin',(14.,0.,1.5));
#19314=CARTESIAN_POINT('Origin',(14.,0.,0.97));
#19315=CARTESIAN_POINT('',(13.775,-2.75545529808154E-17,0.97));
#19316=CARTESIAN_POINT('Origin',(14.,0.,0.97));
#19317=CARTESIAN_POINT('Origin',(8.,0.,0.97));
#19318=CARTESIAN_POINT('',(7.625,-4.59242549680257E-17,0.97));
#19319=CARTESIAN_POINT('Origin',(8.,0.,0.97));
#19320=CARTESIAN_POINT('',(7.625,4.59242549680257E-17,1.5));
#19321=CARTESIAN_POINT('',(7.625,-4.59242549680257E-17,0.97));
#19322=CARTESIAN_POINT('Origin',(8.,0.,1.5));
#19323=CARTESIAN_POINT('Origin',(8.,0.,0.97));
#19324=CARTESIAN_POINT('',(7.775,-2.75545529808154E-17,0.97));
#19325=CARTESIAN_POINT('Origin',(8.,0.,0.97));
#19326=CARTESIAN_POINT('Origin',(2.,0.,0.97));
#19327=CARTESIAN_POINT('',(1.625,-4.59242549680257E-17,0.97));
#19328=CARTESIAN_POINT('Origin',(2.,0.,0.97));
#19329=CARTESIAN_POINT('',(1.625,4.59242549680257E-17,1.5));
#19330=CARTESIAN_POINT('',(1.625,-4.59242549680257E-17,0.97));
#19331=CARTESIAN_POINT('Origin',(2.,0.,1.5));
#19332=CARTESIAN_POINT('Origin',(2.,0.,0.97));
#19333=CARTESIAN_POINT('',(1.775,-2.75545529808155E-17,0.97));
#19334=CARTESIAN_POINT('Origin',(2.,0.,0.97));
#19335=CARTESIAN_POINT('Origin',(20.,0.,0.97));
#19336=CARTESIAN_POINT('',(19.625,-4.59242549680257E-17,0.97));
#19337=CARTESIAN_POINT('Origin',(20.,0.,0.97));
#19338=CARTESIAN_POINT('',(19.625,4.59242549680257E-17,1.5));
#19339=CARTESIAN_POINT('',(19.625,-4.59242549680257E-17,0.97));
#19340=CARTESIAN_POINT('Origin',(20.,0.,1.5));
#19341=CARTESIAN_POINT('Origin',(20.,0.,0.97));
#19342=CARTESIAN_POINT('',(19.775,-2.75545529808156E-17,0.97));
#19343=CARTESIAN_POINT('Origin',(20.,0.,0.97));
#19344=CARTESIAN_POINT('Origin',(14.,0.,-0.1));
#19345=CARTESIAN_POINT('',(13.775,-2.75545529808154E-17,0.));
#19346=CARTESIAN_POINT('Origin',(14.,0.,0.));
#19347=CARTESIAN_POINT('',(13.775,-2.75545529808154E-17,-0.1));
#19348=CARTESIAN_POINT('Origin',(8.,0.,-0.1));
#19349=CARTESIAN_POINT('',(7.775,-2.75545529808154E-17,0.));
#19350=CARTESIAN_POINT('Origin',(8.,0.,0.));
#19351=CARTESIAN_POINT('',(7.775,-2.75545529808154E-17,-0.1));
#19352=CARTESIAN_POINT('Origin',(2.,0.,-0.1));
#19353=CARTESIAN_POINT('',(1.775,-2.75545529808155E-17,0.));
#19354=CARTESIAN_POINT('Origin',(2.,0.,0.));
#19355=CARTESIAN_POINT('',(1.775,-2.75545529808155E-17,-0.1));
#19356=CARTESIAN_POINT('Origin',(20.,0.,-0.1));
#19357=CARTESIAN_POINT('',(19.775,-2.75545529808156E-17,0.));
#19358=CARTESIAN_POINT('Origin',(20.,0.,0.));
#19359=CARTESIAN_POINT('',(19.775,-2.75545529808156E-17,-0.1));
#19360=CARTESIAN_POINT('Origin',(0.,-0.53,1.));
#19361=CARTESIAN_POINT('',(0.,-0.53,1.));
#19362=CARTESIAN_POINT('',(0.,-0.75,0.85));
#19363=CARTESIAN_POINT('',(0.,-0.53,1.));
#19364=CARTESIAN_POINT('',(22.,-0.75,0.85));
#19365=CARTESIAN_POINT('',(0.,-0.75,0.85));
#19366=CARTESIAN_POINT('',(22.,-0.53,1.));
#19367=CARTESIAN_POINT('',(22.,-0.53,1.));
#19368=CARTESIAN_POINT('',(0.,-0.53,1.));
#19369=CARTESIAN_POINT('Origin',(0.,-0.53,1.15));
#19370=CARTESIAN_POINT('',(0.,-0.53,1.15));
#19371=CARTESIAN_POINT('',(0.,-0.53,1.15));
#19372=CARTESIAN_POINT('',(22.,-0.53,1.15));
#19373=CARTESIAN_POINT('',(22.,-0.53,1.15));
#19374=CARTESIAN_POINT('',(0.,-0.53,1.15));
#19375=CARTESIAN_POINT('Origin',(0.,-0.75,1.3));
#19376=CARTESIAN_POINT('',(0.,-0.75,1.3));
#19377=CARTESIAN_POINT('',(0.,-0.75,1.3));
#19378=CARTESIAN_POINT('',(22.,-0.75,1.3));
#19379=CARTESIAN_POINT('',(22.,-0.75,1.3));
#19380=CARTESIAN_POINT('',(0.,-0.75,1.3));
#19381=CARTESIAN_POINT('Origin',(0.,-0.75,1.5));
#19382=CARTESIAN_POINT('',(0.,-0.75,1.5));
#19383=CARTESIAN_POINT('',(0.,-0.75,1.5));
#19384=CARTESIAN_POINT('',(22.,-0.75,1.5));
#19385=CARTESIAN_POINT('',(22.,-0.75,1.5));
#19386=CARTESIAN_POINT('',(0.,-0.75,1.5));
#19387=CARTESIAN_POINT('Origin',(0.,0.75,1.5));
#19388=CARTESIAN_POINT('',(0.,0.75,1.5));
#19389=CARTESIAN_POINT('',(0.,0.75,1.5));
#19390=CARTESIAN_POINT('',(22.,0.75,1.5));
#19391=CARTESIAN_POINT('',(22.,0.75,1.5));
#19392=CARTESIAN_POINT('',(0.,0.75,1.5));
#19393=CARTESIAN_POINT('Origin',(0.,0.75,1.3));
#19394=CARTESIAN_POINT('',(0.,0.75,1.3));
#19395=CARTESIAN_POINT('',(0.,0.75,1.3));
#19396=CARTESIAN_POINT('',(22.,0.75,1.3));
#19397=CARTESIAN_POINT('',(22.,0.75,1.3));
#19398=CARTESIAN_POINT('',(0.,0.75,1.3));
#19399=CARTESIAN_POINT('Origin',(0.,0.53,1.15));
#19400=CARTESIAN_POINT('',(0.,0.53,1.15));
#19401=CARTESIAN_POINT('',(0.,0.53,1.15));
#19402=CARTESIAN_POINT('',(22.,0.53,1.15));
#19403=CARTESIAN_POINT('',(22.,0.53,1.15));
#19404=CARTESIAN_POINT('',(0.,0.53,1.15));
#19405=CARTESIAN_POINT('Origin',(0.,0.53,1.));
#19406=CARTESIAN_POINT('',(0.,0.53,1.));
#19407=CARTESIAN_POINT('',(0.,0.53,1.));
#19408=CARTESIAN_POINT('',(22.,0.53,1.));
#19409=CARTESIAN_POINT('',(22.,0.53,1.));
#19410=CARTESIAN_POINT('',(0.,0.53,1.));
#19411=CARTESIAN_POINT('Origin',(0.,0.75,0.85));
#19412=CARTESIAN_POINT('',(0.,0.75,0.85));
#19413=CARTESIAN_POINT('',(0.,0.75,0.85));
#19414=CARTESIAN_POINT('',(22.,0.75,0.85));
#19415=CARTESIAN_POINT('',(22.,0.75,0.85));
#19416=CARTESIAN_POINT('',(0.,0.75,0.85));
#19417=CARTESIAN_POINT('Origin',(0.,0.75,0.));
#19418=CARTESIAN_POINT('',(0.,0.75,0.));
#19419=CARTESIAN_POINT('',(0.,0.75,0.));
#19420=CARTESIAN_POINT('',(22.,0.75,0.));
#19421=CARTESIAN_POINT('',(22.,0.75,0.));
#19422=CARTESIAN_POINT('',(0.,0.75,0.));
#19423=CARTESIAN_POINT('Origin',(0.,-0.75,0.));
#19424=CARTESIAN_POINT('',(0.,-0.75,0.));
#19425=CARTESIAN_POINT('',(0.,-0.75,0.));
#19426=CARTESIAN_POINT('',(22.,-0.75,0.));
#19427=CARTESIAN_POINT('',(22.,-0.75,0.));
#19428=CARTESIAN_POINT('',(0.,-0.75,0.));
#19429=CARTESIAN_POINT('Origin',(0.,-0.75,0.85));
#19430=CARTESIAN_POINT('',(0.,-0.75,0.85));
#19431=CARTESIAN_POINT('',(22.,-0.75,0.85));
#19432=CARTESIAN_POINT('Origin',(22.,0.,0.75));
#19433=CARTESIAN_POINT('Origin',(0.,0.,0.75));
#19434=CARTESIAN_POINT('',(0.,0.,0.));
#19435=CARTESIAN_POINT('',(0.,0.,0.));
#19436=CARTESIAN_POINT('Origin',(0.,0.,0.));
#19437=CARTESIAN_POINT('',(-0.976185,-0.246528389340863,-1.19548183562566E-16));
#19438=CARTESIAN_POINT('',(-1.19548183562566E-16,-0.246528389340863,0.976185));
#19439=CARTESIAN_POINT('Origin',(0.,-0.246528389340863,0.));
#19440=CARTESIAN_POINT('Origin',(0.,-0.246528389340863,0.));
#19441=CARTESIAN_POINT('',(-1.19548183562566E-16,0.246528389340863,0.976185));
#19442=CARTESIAN_POINT('Origin',(-1.22464679914735E-16,0.,1.));
#19443=CARTESIAN_POINT('',(-0.976185,0.246528389340863,1.19548183562566E-16));
#19444=CARTESIAN_POINT('Origin',(0.,0.246528389340863,0.));
#19445=CARTESIAN_POINT('Origin',(0.,0.246528389340863,0.));
#19446=CARTESIAN_POINT('Origin',(0.,0.,0.));
#19447=CARTESIAN_POINT('',(-0.976185,0.45,-1.19548183562566E-16));
#19448=CARTESIAN_POINT('',(-0.976185,0.,-1.19548183562566E-16));
#19449=CARTESIAN_POINT('Origin',(0.,0.45,0.));
#19450=CARTESIAN_POINT('Origin',(0.,0.,0.));
#19451=CARTESIAN_POINT('',(-0.5,-0.39,-6.12323399573677E-17));
#19452=CARTESIAN_POINT('Origin',(0.,-0.39,0.));
#19453=CARTESIAN_POINT('',(-0.5,0.39,-6.12323399573677E-17));
#19454=CARTESIAN_POINT('',(-0.5,0.,-6.12323399573677E-17));
#19455=CARTESIAN_POINT('Origin',(0.,0.39,0.));
#19456=CARTESIAN_POINT('Origin',(0.,0.42,0.));
#19457=CARTESIAN_POINT('',(-0.56,0.45,-6.85802207522518E-17));
#19458=CARTESIAN_POINT('',(-0.53,0.42,-6.49062803548097E-17));
#19459=CARTESIAN_POINT('Origin',(0.,0.45,0.));
#19460=CARTESIAN_POINT('Origin',(0.976185,0.45,0.));
#19461=CARTESIAN_POINT('Origin',(0.,0.,0.));
#19462=CARTESIAN_POINT('',(-0.976185,-0.45,-1.19548183562566E-16));
#19463=CARTESIAN_POINT('Origin',(0.,-0.45,0.));
#19464=CARTESIAN_POINT('',(-0.976185,0.,-1.19548183562566E-16));
#19465=CARTESIAN_POINT('Origin',(0.56,-0.45,0.));
#19466=CARTESIAN_POINT('',(-0.56,-0.45,-6.85802207522518E-17));
#19467=CARTESIAN_POINT('Origin',(0.,-0.45,0.));
#19468=CARTESIAN_POINT('Origin',(0.,-0.42,0.));
#19469=CARTESIAN_POINT('',(-0.53,-0.42,-6.49062803548097E-17));
#19470=CARTESIAN_POINT('',(0.,0.,0.));
#19471=CARTESIAN_POINT('Origin',(0.,0.,0.));
#19472=CARTESIAN_POINT('',(-1.023815,0.246528389340863,-1.25381176266905E-16));
#19473=CARTESIAN_POINT('',(-1.25381176266905E-16,0.246528389340863,1.023815));
#19474=CARTESIAN_POINT('Origin',(0.,0.246528389340863,0.));
#19475=CARTESIAN_POINT('Origin',(0.,0.246528389340863,0.));
#19476=CARTESIAN_POINT('',(-1.25381176266905E-16,-0.246528389340863,1.023815));
#19477=CARTESIAN_POINT('Origin',(-1.22464679914735E-16,0.,1.));
#19478=CARTESIAN_POINT('',(-1.023815,-0.246528389340863,1.25381176266905E-16));
#19479=CARTESIAN_POINT('Origin',(0.,-0.246528389340863,0.));
#19480=CARTESIAN_POINT('Origin',(0.,-0.246528389340863,0.));
#19481=CARTESIAN_POINT('Origin',(0.,0.,0.));
#19482=CARTESIAN_POINT('',(-1.023815,-0.45,-1.25381176266905E-16));
#19483=CARTESIAN_POINT('Origin',(0.,-0.45,0.));
#19484=CARTESIAN_POINT('',(-1.023815,0.,-1.25381176266905E-16));
#19485=CARTESIAN_POINT('Origin',(1.44,0.45,0.));
#19486=CARTESIAN_POINT('',(-1.44,0.45,-1.76349139077219E-16));
#19487=CARTESIAN_POINT('Origin',(0.,0.45,0.));
#19488=CARTESIAN_POINT('',(-1.023815,0.45,-1.25381176266905E-16));
#19489=CARTESIAN_POINT('Origin',(0.,0.45,0.));
#19490=CARTESIAN_POINT('Origin',(0.,0.42,0.));
#19491=CARTESIAN_POINT('',(-1.5,0.39,-1.83697019872103E-16));
#19492=CARTESIAN_POINT('Origin',(0.,0.39,0.));
#19493=CARTESIAN_POINT('',(-1.47,0.42,-1.80023079474661E-16));
#19494=CARTESIAN_POINT('Origin',(0.,0.,0.));
#19495=CARTESIAN_POINT('',(-1.5,-0.39,-1.83697019872103E-16));
#19496=CARTESIAN_POINT('Origin',(0.,-0.39,0.));
#19497=CARTESIAN_POINT('',(-1.5,0.,-1.83697019872103E-16));
#19498=CARTESIAN_POINT('Origin',(0.,-0.42,0.));
#19499=CARTESIAN_POINT('',(-1.44,-0.45,-1.76349139077219E-16));
#19500=CARTESIAN_POINT('Origin',(0.,-0.45,0.));
#19501=CARTESIAN_POINT('',(-1.47,-0.42,-1.80023079474661E-16));
#19502=CARTESIAN_POINT('Origin',(1.023815,-0.45,0.));
#19503=CARTESIAN_POINT('Origin',(0.,0.,0.));
#19504=CARTESIAN_POINT('',(-1.023815,0.,-1.25381176266905E-16));
#19505=CARTESIAN_POINT('',(0.,0.,0.));
#19506=CARTESIAN_POINT('Origin',(1.,0.,0.));
#19507=CARTESIAN_POINT('',(1.,-1.78583896120461E-33,0.23815));
#19508=CARTESIAN_POINT('',(1.,-1.78583896120461E-33,-0.23815));
#19509=CARTESIAN_POINT('Origin',(1.,0.,0.));
#19510=CARTESIAN_POINT('Origin',(0.707106781186548,0.,-0.707106781186547));
#19511=CARTESIAN_POINT('',(0.875504261126124,-1.78583896120461E-33,-0.538709301246971));
#19512=CARTESIAN_POINT('',(0.538709301246971,-1.78583896120461E-33,-0.875504261126124));
#19513=CARTESIAN_POINT('Origin',(0.707106781186548,0.,-0.707106781186547));
#19514=CARTESIAN_POINT('Origin',(6.12323399573677E-17,0.,-1.));
#19515=CARTESIAN_POINT('',(0.23815,-1.78583896120461E-33,-1.));
#19516=CARTESIAN_POINT('',(-0.23815,-1.78583896120461E-33,-1.));
#19517=CARTESIAN_POINT('Origin',(6.12323399573677E-17,0.,-1.));
#19518=CARTESIAN_POINT('Origin',(-0.707106781186547,0.,-0.707106781186548));
#19519=CARTESIAN_POINT('',(-0.538709301246971,-1.78583896120461E-33,-0.875504261126124));
#19520=CARTESIAN_POINT('',(-0.875504261126124,-1.78583896120461E-33,-0.538709301246971));
#19521=CARTESIAN_POINT('Origin',(-0.707106781186547,0.,-0.707106781186548));
#19522=CARTESIAN_POINT('Origin',(-1.,0.,-1.22464679914735E-16));
#19523=CARTESIAN_POINT('',(-1.,-1.78583896120461E-33,-0.23815));
#19524=CARTESIAN_POINT('',(-1.,-1.78583896120461E-33,0.23815));
#19525=CARTESIAN_POINT('Origin',(-1.,0.,-1.22464679914735E-16));
#19526=CARTESIAN_POINT('Origin',(-0.707106781186548,0.,0.707106781186547));
#19527=CARTESIAN_POINT('',(-0.875504261126124,-7.94881478324376E-33,0.538709301246971));
#19528=CARTESIAN_POINT('',(-0.538709301246971,4.37713686083455E-33,0.875504261126124));
#19529=CARTESIAN_POINT('Origin',(-0.707106781186548,0.,0.707106781186547));
#19530=CARTESIAN_POINT('Origin',(-1.83697019872103E-16,0.,1.));
#19531=CARTESIAN_POINT('',(-0.23815,-1.78583896120461E-33,1.));
#19532=CARTESIAN_POINT('',(0.23815,-1.78583896120461E-33,1.));
#19533=CARTESIAN_POINT('Origin',(-1.83697019872103E-16,0.,1.));
#19534=CARTESIAN_POINT('Origin',(0.707106781186547,0.,0.707106781186548));
#19535=CARTESIAN_POINT('',(0.538709301246971,-4.86732687222419E-33,0.875504261126124));
#19536=CARTESIAN_POINT('',(0.875504261126124,1.29564894981497E-33,0.538709301246971));
#19537=CARTESIAN_POINT('Origin',(0.707106781186547,0.,0.707106781186548));
#19538=CARTESIAN_POINT('',(0.,0.,0.));
#19539=CARTESIAN_POINT('Origin',(0.707106781186547,0.,0.707106781186548));
#19540=CARTESIAN_POINT('',(0.504455939115715,-0.04763,0.841298510752802));
#19541=CARTESIAN_POINT('',(0.841298510752802,-0.04763,0.504455939115715));
#19542=CARTESIAN_POINT('Ctrl Pts',(0.504455939115715,-0.04763,0.841298510752802));
#19543=CARTESIAN_POINT('Ctrl Pts',(0.508899795931835,-0.0740444353928835,
0.838633903678357));
#19544=CARTESIAN_POINT('Ctrl Pts',(0.517157748491652,-0.0999305678883309,
0.833661031856294));
#19545=CARTESIAN_POINT('Ctrl Pts',(0.537715343527944,-0.142345102874864,
0.820511285096538));
#19546=CARTESIAN_POINT('Ctrl Pts',(0.548874290046456,-0.159766064500479,
0.813159949759));
#19547=CARTESIAN_POINT('Ctrl Pts',(0.573915184558107,-0.190326085855194,
0.795684265985089));
#19548=CARTESIAN_POINT('Ctrl Pts',(0.587792702767295,-0.203463743702801,
0.78555112003688));
#19549=CARTESIAN_POINT('Ctrl Pts',(0.615966552324775,-0.224161999508995,
0.763642258217233));
#19550=CARTESIAN_POINT('Ctrl Pts',(0.631684198665438,-0.232861760990032,
0.750785745543687));
#19551=CARTESIAN_POINT('Ctrl Pts',(0.663382628119203,-0.244251601209411,
0.722929908501543));
#19552=CARTESIAN_POINT('Ctrl Pts',(0.679352081686668,-0.246942143572133,
0.707917883896095));
#19553=CARTESIAN_POINT('Ctrl Pts',(0.707917883896095,-0.246942143572133,
0.679352081686668));
#19554=CARTESIAN_POINT('Ctrl Pts',(0.722929908501543,-0.244251601209411,
0.663382628119203));
#19555=CARTESIAN_POINT('Ctrl Pts',(0.750785745543687,-0.232861760990032,
0.631684198665439));
#19556=CARTESIAN_POINT('Ctrl Pts',(0.763642258217232,-0.224161999508995,
0.615966552324775));
#19557=CARTESIAN_POINT('Ctrl Pts',(0.78555112003688,-0.203463743702801,
0.587792702767295));
#19558=CARTESIAN_POINT('Ctrl Pts',(0.795684265985088,-0.190326085855194,
0.573915184558108));
#19559=CARTESIAN_POINT('Ctrl Pts',(0.813159949759,-0.15976606450048,0.548874290046456));
#19560=CARTESIAN_POINT('Ctrl Pts',(0.820511285096538,-0.142345102874864,
0.537715343527944));
#19561=CARTESIAN_POINT('Ctrl Pts',(0.833661031856294,-0.099930567888331,
0.517157748491653));
#19562=CARTESIAN_POINT('Ctrl Pts',(0.838633903678357,-0.0740444353928835,
0.508899795931835));
#19563=CARTESIAN_POINT('Ctrl Pts',(0.841298510752801,-0.0476299999999999,
0.504455939115715));
#19564=CARTESIAN_POINT('',(0.528110872004958,-0.04763,0.871530771444223));
#19565=CARTESIAN_POINT('Origin',(0.707106781186547,-0.04763,0.707106781186548));
#19566=CARTESIAN_POINT('',(0.871530771444223,-0.04763,0.528110872004959));
#19567=CARTESIAN_POINT('Ctrl Pts',(0.871530771444223,-0.0476300000000001,
0.528110872004958));
#19568=CARTESIAN_POINT('Ctrl Pts',(0.87014664509073,-0.0609922781173483,
0.530395067942936));
#19569=CARTESIAN_POINT('Ctrl Pts',(0.868149331745851,-0.0742967091364493,
0.533674141594226));
#19570=CARTESIAN_POINT('Ctrl Pts',(0.85981294420286,-0.115492077056649,
0.54708917182331));
#19571=CARTESIAN_POINT('Ctrl Pts',(0.850993704737257,-0.141695629206859,
0.560922177770136));
#19572=CARTESIAN_POINT('Ctrl Pts',(0.830754510485543,-0.181890537957859,
0.590422647829571));
#19573=CARTESIAN_POINT('Ctrl Pts',(0.816896541396381,-0.201072148666545,
0.609616703125488));
#19574=CARTESIAN_POINT('Ctrl Pts',(0.792310597819928,-0.223955109275652,
0.641117951819998));
#19575=CARTESIAN_POINT('Ctrl Pts',(0.779109323683612,-0.232742381310829,
0.657208095763053));
#19576=CARTESIAN_POINT('Ctrl Pts',(0.750552691816206,-0.244234834628584,
0.68964083160521));
#19577=CARTESIAN_POINT('Ctrl Pts',(0.735185187071673,-0.246942143572133,
0.705971972091755));
#19578=CARTESIAN_POINT('Ctrl Pts',(0.705971972091754,-0.246942143572133,
0.735185187071673));
#19579=CARTESIAN_POINT('Ctrl Pts',(0.689640831605209,-0.244234834628584,
0.750552691816206));
#19580=CARTESIAN_POINT('Ctrl Pts',(0.657208095763052,-0.232742381310829,
0.779109323683612));
#19581=CARTESIAN_POINT('Ctrl Pts',(0.641117951819998,-0.223955109275652,
0.792310597819928));
#19582=CARTESIAN_POINT('Ctrl Pts',(0.609616703125487,-0.201072148666545,
0.816896541396382));
#19583=CARTESIAN_POINT('Ctrl Pts',(0.590422647829571,-0.181890537957858,
0.830754510485544));
#19584=CARTESIAN_POINT('Ctrl Pts',(0.560922177770135,-0.141695629206858,
0.850993704737257));
#19585=CARTESIAN_POINT('Ctrl Pts',(0.547089171823309,-0.115492077056649,
0.859812944202861));
#19586=CARTESIAN_POINT('Ctrl Pts',(0.533674141594226,-0.0742967091364491,
0.868149331745852));
#19587=CARTESIAN_POINT('Ctrl Pts',(0.530395067942936,-0.0609922781173483,
0.870146645090731));
#19588=CARTESIAN_POINT('Ctrl Pts',(0.528110872004958,-0.0476300000000001,
0.871530771444223));
#19589=CARTESIAN_POINT('Origin',(0.707106781186547,-0.04763,0.707106781186548));
#19590=CARTESIAN_POINT('Origin',(0.,-0.166705,0.));
#19591=CARTESIAN_POINT('',(0.242834539687906,-0.04763,0.989696097314));
#19592=CARTESIAN_POINT('Origin',(0.,-0.04763,0.));
#19593=CARTESIAN_POINT('',(-0.242834539687907,-0.04763,0.989696097314));
#19594=CARTESIAN_POINT('Ctrl Pts',(0.242834539687906,-0.04763,0.989696097314));
#19595=CARTESIAN_POINT('Ctrl Pts',(0.24024064412003,-0.0609922781173483,
0.990332542620729));
#19596=CARTESIAN_POINT('Ctrl Pts',(0.236509675094874,-0.0742967091364492,
0.991238884025248));
#19597=CARTESIAN_POINT('Ctrl Pts',(0.221129100087819,-0.115492077056649,
0.994830026707808));
#19598=CARTESIAN_POINT('Ctrl Pts',(0.205111543747588,-0.141695629206859,
0.998375294985966));
#19599=CARTESIAN_POINT('Ctrl Pts',(0.169940289819232,-0.181890537957859,
1.00492400591205));
#19600=CARTESIAN_POINT('Ctrl Pts',(0.1465689792446,-0.201072148666545,1.00869718865384));
#19601=CARTESIAN_POINT('Ctrl Pts',(0.106909345252087,-0.223955109275652,
1.01358704779679));
#19602=CARTESIAN_POINT('Ctrl Pts',(0.0861971848975941,-0.232742381310829,
1.0156297872271));
#19603=CARTESIAN_POINT('Ctrl Pts',(0.0430711894098822,-0.244234834628584,
1.01837060663223));
#19604=CARTESIAN_POINT('Ctrl Pts',(0.0206568624125605,-0.246942143572133,
1.019052));
#19605=CARTESIAN_POINT('Ctrl Pts',(-0.0206568624125608,-0.246942143572133,
1.019052));
#19606=CARTESIAN_POINT('Ctrl Pts',(-0.0430711894098825,-0.244234834628584,
1.01837060663223));
#19607=CARTESIAN_POINT('Ctrl Pts',(-0.0861971848975943,-0.232742381310829,
1.0156297872271));
#19608=CARTESIAN_POINT('Ctrl Pts',(-0.106909345252088,-0.223955109275652,
1.01358704779679));
#19609=CARTESIAN_POINT('Ctrl Pts',(-0.1465689792446,-0.201072148666545,
1.00869718865384));
#19610=CARTESIAN_POINT('Ctrl Pts',(-0.169940289819232,-0.181890537957859,
1.00492400591205));
#19611=CARTESIAN_POINT('Ctrl Pts',(-0.205111543747588,-0.141695629206859,
0.998375294985966));
#19612=CARTESIAN_POINT('Ctrl Pts',(-0.221129100087819,-0.115492077056649,
0.994830026707808));
#19613=CARTESIAN_POINT('Ctrl Pts',(-0.236509675094875,-0.0742967091364493,
0.991238884025248));
#19614=CARTESIAN_POINT('Ctrl Pts',(-0.24024064412003,-0.0609922781173483,
0.990332542620729));
#19615=CARTESIAN_POINT('Ctrl Pts',(-0.242834539687907,-0.04763,0.989696097314));
#19616=CARTESIAN_POINT('',(-0.528110872004959,-0.04763,0.871530771444223));
#19617=CARTESIAN_POINT('Origin',(0.,-0.04763,0.));
#19618=CARTESIAN_POINT('',(-0.871530771444223,-0.04763,0.528110872004958));
#19619=CARTESIAN_POINT('Ctrl Pts',(-0.528110872004958,-0.0476300000000001,
0.871530771444223));
#19620=CARTESIAN_POINT('Ctrl Pts',(-0.530395067942936,-0.0609922781173484,
0.87014664509073));
#19621=CARTESIAN_POINT('Ctrl Pts',(-0.533674141594226,-0.0742967091364493,
0.868149331745851));
#19622=CARTESIAN_POINT('Ctrl Pts',(-0.54708917182331,-0.115492077056649,
0.85981294420286));
#19623=CARTESIAN_POINT('Ctrl Pts',(-0.560922177770136,-0.141695629206859,
0.850993704737257));
#19624=CARTESIAN_POINT('Ctrl Pts',(-0.590422647829571,-0.181890537957859,
0.830754510485543));
#19625=CARTESIAN_POINT('Ctrl Pts',(-0.609616703125488,-0.201072148666545,
0.816896541396381));
#19626=CARTESIAN_POINT('Ctrl Pts',(-0.641117951819998,-0.223955109275652,
0.792310597819928));
#19627=CARTESIAN_POINT('Ctrl Pts',(-0.657208095763053,-0.232742381310829,
0.779109323683611));
#19628=CARTESIAN_POINT('Ctrl Pts',(-0.68964083160521,-0.244234834628584,
0.750552691816205));
#19629=CARTESIAN_POINT('Ctrl Pts',(-0.705971972091755,-0.246942143572133,
0.735185187071673));
#19630=CARTESIAN_POINT('Ctrl Pts',(-0.735185187071673,-0.246942143572133,
0.705971972091754));
#19631=CARTESIAN_POINT('Ctrl Pts',(-0.750552691816206,-0.244234834628584,
0.689640831605209));
#19632=CARTESIAN_POINT('Ctrl Pts',(-0.779109323683612,-0.232742381310829,
0.657208095763052));
#19633=CARTESIAN_POINT('Ctrl Pts',(-0.792310597819928,-0.223955109275652,
0.641117951819998));
#19634=CARTESIAN_POINT('Ctrl Pts',(-0.816896541396382,-0.201072148666545,
0.609616703125487));
#19635=CARTESIAN_POINT('Ctrl Pts',(-0.830754510485544,-0.181890537957858,
0.590422647829571));
#19636=CARTESIAN_POINT('Ctrl Pts',(-0.850993704737257,-0.141695629206858,
0.560922177770135));
#19637=CARTESIAN_POINT('Ctrl Pts',(-0.859812944202861,-0.115492077056649,
0.547089171823309));
#19638=CARTESIAN_POINT('Ctrl Pts',(-0.868149331745852,-0.0742967091364491,
0.533674141594226));
#19639=CARTESIAN_POINT('Ctrl Pts',(-0.870146645090731,-0.0609922781173483,
0.530395067942936));
#19640=CARTESIAN_POINT('Ctrl Pts',(-0.871530771444223,-0.04763,0.528110872004958));
#19641=CARTESIAN_POINT('',(-0.989696097314,-0.04763,0.242834539687906));
#19642=CARTESIAN_POINT('Origin',(0.,-0.04763,0.));
#19643=CARTESIAN_POINT('',(-1.019052,-0.246942143572133,1.248489836334E-16));
#19644=CARTESIAN_POINT('Ctrl Pts',(-0.989696097314,-0.04763,0.242834539687906));
#19645=CARTESIAN_POINT('Ctrl Pts',(-0.990332542620729,-0.0609922781173483,
0.24024064412003));
#19646=CARTESIAN_POINT('Ctrl Pts',(-0.991238884025248,-0.0742967091364492,
0.236509675094874));
#19647=CARTESIAN_POINT('Ctrl Pts',(-0.994830026707808,-0.115492077056649,
0.221129100087819));
#19648=CARTESIAN_POINT('Ctrl Pts',(-0.998375294985966,-0.141695629206859,
0.205111543747588));
#19649=CARTESIAN_POINT('Ctrl Pts',(-1.00492400591205,-0.181890537957859,
0.169940289819232));
#19650=CARTESIAN_POINT('Ctrl Pts',(-1.00869718865384,-0.201072148666545,
0.1465689792446));
#19651=CARTESIAN_POINT('Ctrl Pts',(-1.01358704779679,-0.223955109275652,
0.106909345252088));
#19652=CARTESIAN_POINT('Ctrl Pts',(-1.0156297872271,-0.232742381310829,
0.0861971848975944));
#19653=CARTESIAN_POINT('Ctrl Pts',(-1.01837060663223,-0.244234834628584,
0.0430711894098825));
#19654=CARTESIAN_POINT('Ctrl Pts',(-1.019052,-0.246942143572133,0.0206568624125608));
#19655=CARTESIAN_POINT('Ctrl Pts',(-1.019052,-0.246942143572133,1.2490009027033E-16));
#19656=CARTESIAN_POINT('',(-1.019052,-0.28578,1.24797876996471E-16));
#19657=CARTESIAN_POINT('',(-1.019052,-0.166705,1.24797876996471E-16));
#19658=CARTESIAN_POINT('Origin',(0.,-0.28578,0.));
#19659=CARTESIAN_POINT('',(-0.989696097314,-0.04763,-0.242834539687906));
#19660=CARTESIAN_POINT('Ctrl Pts',(-1.019052,-0.246942143572133,1.2490009027033E-16));
#19661=CARTESIAN_POINT('Ctrl Pts',(-1.019052,-0.246942143572133,-0.0206568624125605));
#19662=CARTESIAN_POINT('Ctrl Pts',(-1.01837060663223,-0.244234834628584,
-0.0430711894098822));
#19663=CARTESIAN_POINT('Ctrl Pts',(-1.0156297872271,-0.232742381310829,
-0.0861971848975941));
#19664=CARTESIAN_POINT('Ctrl Pts',(-1.01358704779679,-0.223955109275652,
-0.106909345252087));
#19665=CARTESIAN_POINT('Ctrl Pts',(-1.00869718865384,-0.201072148666546,
-0.1465689792446));
#19666=CARTESIAN_POINT('Ctrl Pts',(-1.00492400591205,-0.181890537957859,
-0.169940289819232));
#19667=CARTESIAN_POINT('Ctrl Pts',(-0.998375294985966,-0.141695629206859,
-0.205111543747588));
#19668=CARTESIAN_POINT('Ctrl Pts',(-0.994830026707808,-0.11549207705665,
-0.221129100087819));
#19669=CARTESIAN_POINT('Ctrl Pts',(-0.991238884025248,-0.0742967091364495,
-0.236509675094874));
#19670=CARTESIAN_POINT('Ctrl Pts',(-0.990332542620729,-0.0609922781173484,
-0.24024064412003));
#19671=CARTESIAN_POINT('Ctrl Pts',(-0.989696097314,-0.0476300000000001,
-0.242834539687907));
#19672=CARTESIAN_POINT('',(-0.871530771444223,-0.04763,-0.528110872004958));
#19673=CARTESIAN_POINT('Origin',(0.,-0.04763,0.));
#19674=CARTESIAN_POINT('',(-0.528110872004958,-0.04763,-0.871530771444223));
#19675=CARTESIAN_POINT('Ctrl Pts',(-0.871530771444223,-0.0476300000000001,
-0.528110872004958));
#19676=CARTESIAN_POINT('Ctrl Pts',(-0.87014664509073,-0.0609922781173484,
-0.530395067942936));
#19677=CARTESIAN_POINT('Ctrl Pts',(-0.868149331745851,-0.0742967091364494,
-0.533674141594226));
#19678=CARTESIAN_POINT('Ctrl Pts',(-0.85981294420286,-0.115492077056649,
-0.54708917182331));
#19679=CARTESIAN_POINT('Ctrl Pts',(-0.850993704737257,-0.141695629206859,
-0.560922177770136));
#19680=CARTESIAN_POINT('Ctrl Pts',(-0.830754510485543,-0.181890537957859,
-0.590422647829571));
#19681=CARTESIAN_POINT('Ctrl Pts',(-0.816896541396381,-0.201072148666546,
-0.609616703125488));
#19682=CARTESIAN_POINT('Ctrl Pts',(-0.792310597819928,-0.223955109275652,
-0.641117951819999));
#19683=CARTESIAN_POINT('Ctrl Pts',(-0.779109323683611,-0.232742381310829,
-0.657208095763053));
#19684=CARTESIAN_POINT('Ctrl Pts',(-0.750552691816205,-0.244234834628584,
-0.68964083160521));
#19685=CARTESIAN_POINT('Ctrl Pts',(-0.735185187071673,-0.246942143572133,
-0.705971972091755));
#19686=CARTESIAN_POINT('Ctrl Pts',(-0.705971972091754,-0.246942143572133,
-0.735185187071673));
#19687=CARTESIAN_POINT('Ctrl Pts',(-0.68964083160521,-0.244234834628584,
-0.750552691816206));
#19688=CARTESIAN_POINT('Ctrl Pts',(-0.657208095763052,-0.232742381310829,
-0.779109323683612));
#19689=CARTESIAN_POINT('Ctrl Pts',(-0.641117951819998,-0.223955109275652,
-0.792310597819928));
#19690=CARTESIAN_POINT('Ctrl Pts',(-0.609616703125488,-0.201072148666545,
-0.816896541396381));
#19691=CARTESIAN_POINT('Ctrl Pts',(-0.590422647829571,-0.181890537957859,
-0.830754510485543));
#19692=CARTESIAN_POINT('Ctrl Pts',(-0.560922177770136,-0.141695629206859,
-0.850993704737257));
#19693=CARTESIAN_POINT('Ctrl Pts',(-0.54708917182331,-0.115492077056649,
-0.85981294420286));
#19694=CARTESIAN_POINT('Ctrl Pts',(-0.533674141594226,-0.0742967091364494,
-0.868149331745852));
#19695=CARTESIAN_POINT('Ctrl Pts',(-0.530395067942936,-0.0609922781173484,
-0.870146645090731));
#19696=CARTESIAN_POINT('Ctrl Pts',(-0.528110872004958,-0.0476300000000001,
-0.871530771444223));
#19697=CARTESIAN_POINT('',(-0.242834539687906,-0.04763,-0.989696097314));
#19698=CARTESIAN_POINT('Origin',(0.,-0.04763,0.));
#19699=CARTESIAN_POINT('',(0.242834539687906,-0.04763,-0.989696097314));
#19700=CARTESIAN_POINT('Ctrl Pts',(-0.242834539687907,-0.04763,-0.989696097314));
#19701=CARTESIAN_POINT('Ctrl Pts',(-0.24024064412003,-0.0609922781173483,
-0.990332542620729));
#19702=CARTESIAN_POINT('Ctrl Pts',(-0.236509675094874,-0.0742967091364493,
-0.991238884025248));
#19703=CARTESIAN_POINT('Ctrl Pts',(-0.221129100087819,-0.115492077056649,
-0.994830026707808));
#19704=CARTESIAN_POINT('Ctrl Pts',(-0.205111543747588,-0.141695629206859,
-0.998375294985966));
#19705=CARTESIAN_POINT('Ctrl Pts',(-0.169940289819232,-0.181890537957859,
-1.00492400591205));
#19706=CARTESIAN_POINT('Ctrl Pts',(-0.1465689792446,-0.201072148666545,
-1.00869718865384));
#19707=CARTESIAN_POINT('Ctrl Pts',(-0.106909345252087,-0.223955109275652,
-1.01358704779679));
#19708=CARTESIAN_POINT('Ctrl Pts',(-0.0861971848975942,-0.232742381310829,
-1.0156297872271));
#19709=CARTESIAN_POINT('Ctrl Pts',(-0.0430711894098823,-0.244234834628584,
-1.01837060663223));
#19710=CARTESIAN_POINT('Ctrl Pts',(-0.0206568624125606,-0.246942143572133,
-1.019052));
#19711=CARTESIAN_POINT('Ctrl Pts',(0.0206568624125607,-0.246942143572133,
-1.019052));
#19712=CARTESIAN_POINT('Ctrl Pts',(0.0430711894098824,-0.244234834628584,
-1.01837060663223));
#19713=CARTESIAN_POINT('Ctrl Pts',(0.0861971848975943,-0.232742381310829,
-1.0156297872271));
#19714=CARTESIAN_POINT('Ctrl Pts',(0.106909345252088,-0.223955109275652,
-1.01358704779679));
#19715=CARTESIAN_POINT('Ctrl Pts',(0.1465689792446,-0.201072148666545,-1.00869718865384));
#19716=CARTESIAN_POINT('Ctrl Pts',(0.169940289819232,-0.181890537957859,
-1.00492400591205));
#19717=CARTESIAN_POINT('Ctrl Pts',(0.205111543747588,-0.141695629206859,
-0.998375294985966));
#19718=CARTESIAN_POINT('Ctrl Pts',(0.221129100087819,-0.115492077056649,
-0.994830026707808));
#19719=CARTESIAN_POINT('Ctrl Pts',(0.236509675094874,-0.0742967091364493,
-0.991238884025248));
#19720=CARTESIAN_POINT('Ctrl Pts',(0.24024064412003,-0.0609922781173484,
-0.990332542620729));
#19721=CARTESIAN_POINT('Ctrl Pts',(0.242834539687907,-0.04763,-0.989696097314));
#19722=CARTESIAN_POINT('',(0.528110872004958,-0.04763,-0.871530771444223));
#19723=CARTESIAN_POINT('Origin',(0.,-0.04763,0.));
#19724=CARTESIAN_POINT('',(0.871530771444223,-0.04763,-0.528110872004958));
#19725=CARTESIAN_POINT('Ctrl Pts',(0.528110872004958,-0.0476300000000001,
-0.871530771444223));
#19726=CARTESIAN_POINT('Ctrl Pts',(0.530395067942936,-0.0609922781173484,
-0.870146645090731));
#19727=CARTESIAN_POINT('Ctrl Pts',(0.533674141594226,-0.0742967091364493,
-0.868149331745851));
#19728=CARTESIAN_POINT('Ctrl Pts',(0.54708917182331,-0.115492077056649,
-0.85981294420286));
#19729=CARTESIAN_POINT('Ctrl Pts',(0.560922177770136,-0.141695629206859,
-0.850993704737257));
#19730=CARTESIAN_POINT('Ctrl Pts',(0.590422647829571,-0.181890537957859,
-0.830754510485543));
#19731=CARTESIAN_POINT('Ctrl Pts',(0.609616703125488,-0.201072148666545,
-0.816896541396381));
#19732=CARTESIAN_POINT('Ctrl Pts',(0.641117951819998,-0.223955109275652,
-0.792310597819928));
#19733=CARTESIAN_POINT('Ctrl Pts',(0.657208095763053,-0.232742381310829,
-0.779109323683612));
#19734=CARTESIAN_POINT('Ctrl Pts',(0.68964083160521,-0.244234834628584,
-0.750552691816206));
#19735=CARTESIAN_POINT('Ctrl Pts',(0.705971972091755,-0.246942143572133,
-0.735185187071673));
#19736=CARTESIAN_POINT('Ctrl Pts',(0.735185187071673,-0.246942143572133,
-0.705971972091754));
#19737=CARTESIAN_POINT('Ctrl Pts',(0.750552691816206,-0.244234834628584,
-0.68964083160521));
#19738=CARTESIAN_POINT('Ctrl Pts',(0.779109323683612,-0.232742381310829,
-0.657208095763053));
#19739=CARTESIAN_POINT('Ctrl Pts',(0.792310597819928,-0.223955109275652,
-0.641117951819998));
#19740=CARTESIAN_POINT('Ctrl Pts',(0.816896541396381,-0.201072148666545,
-0.609616703125488));
#19741=CARTESIAN_POINT('Ctrl Pts',(0.830754510485543,-0.181890537957859,
-0.590422647829571));
#19742=CARTESIAN_POINT('Ctrl Pts',(0.850993704737257,-0.141695629206859,
-0.560922177770136));
#19743=CARTESIAN_POINT('Ctrl Pts',(0.85981294420286,-0.115492077056649,
-0.54708917182331));
#19744=CARTESIAN_POINT('Ctrl Pts',(0.868149331745851,-0.0742967091364493,
-0.533674141594226));
#19745=CARTESIAN_POINT('Ctrl Pts',(0.870146645090731,-0.0609922781173484,
-0.530395067942936));
#19746=CARTESIAN_POINT('Ctrl Pts',(0.871530771444223,-0.0476300000000001,
-0.528110872004958));
#19747=CARTESIAN_POINT('',(0.989696097314,-0.04763,-0.242834539687906));
#19748=CARTESIAN_POINT('Origin',(0.,-0.04763,0.));
#19749=CARTESIAN_POINT('',(0.989696097314,-0.04763,0.242834539687906));
#19750=CARTESIAN_POINT('Ctrl Pts',(0.989696097314,-0.04763,-0.242834539687907));
#19751=CARTESIAN_POINT('Ctrl Pts',(0.990332542620729,-0.0609922781173483,
-0.24024064412003));
#19752=CARTESIAN_POINT('Ctrl Pts',(0.991238884025248,-0.0742967091364493,
-0.236509675094874));
#19753=CARTESIAN_POINT('Ctrl Pts',(0.994830026707808,-0.115492077056649,
-0.221129100087819));
#19754=CARTESIAN_POINT('Ctrl Pts',(0.998375294985966,-0.141695629206859,
-0.205111543747588));
#19755=CARTESIAN_POINT('Ctrl Pts',(1.00492400591205,-0.181890537957859,
-0.169940289819232));
#19756=CARTESIAN_POINT('Ctrl Pts',(1.00869718865384,-0.201072148666545,
-0.1465689792446));
#19757=CARTESIAN_POINT('Ctrl Pts',(1.01358704779679,-0.223955109275652,
-0.106909345252087));
#19758=CARTESIAN_POINT('Ctrl Pts',(1.0156297872271,-0.232742381310829,-0.0861971848975942));
#19759=CARTESIAN_POINT('Ctrl Pts',(1.01837060663223,-0.244234834628584,
-0.0430711894098823));
#19760=CARTESIAN_POINT('Ctrl Pts',(1.019052,-0.246942143572133,-0.0206568624125607));
#19761=CARTESIAN_POINT('Ctrl Pts',(1.019052,-0.246942143572133,0.0206568624125607));
#19762=CARTESIAN_POINT('Ctrl Pts',(1.01837060663223,-0.244234834628584,
0.0430711894098823));
#19763=CARTESIAN_POINT('Ctrl Pts',(1.0156297872271,-0.232742381310829,0.0861971848975942));
#19764=CARTESIAN_POINT('Ctrl Pts',(1.01358704779679,-0.223955109275652,
0.106909345252087));
#19765=CARTESIAN_POINT('Ctrl Pts',(1.00869718865384,-0.201072148666545,
0.1465689792446));
#19766=CARTESIAN_POINT('Ctrl Pts',(1.00492400591205,-0.181890537957859,
0.169940289819232));
#19767=CARTESIAN_POINT('Ctrl Pts',(0.998375294985966,-0.141695629206859,
0.205111543747588));
#19768=CARTESIAN_POINT('Ctrl Pts',(0.994830026707808,-0.115492077056649,
0.221129100087819));
#19769=CARTESIAN_POINT('Ctrl Pts',(0.991238884025248,-0.0742967091364492,
0.236509675094874));
#19770=CARTESIAN_POINT('Ctrl Pts',(0.990332542620729,-0.0609922781173483,
0.24024064412003));
#19771=CARTESIAN_POINT('Ctrl Pts',(0.989696097314,-0.04763,0.242834539687907));
#19772=CARTESIAN_POINT('Origin',(0.,-0.04763,0.));
#19773=CARTESIAN_POINT('Origin',(0.,-0.04763,0.));
#19774=CARTESIAN_POINT('',(0.238183666596899,-0.04763,0.951592097314));
#19775=CARTESIAN_POINT('Origin',(0.,-0.04763,0.));
#19776=CARTESIAN_POINT('Origin',(-1.94289029309402E-16,-0.04763,1.));
#19777=CARTESIAN_POINT('Origin',(-1.94289029309402E-16,0.,1.));
#19778=CARTESIAN_POINT('',(-0.2381836665969,-0.04763,0.951592097314));
#19779=CARTESIAN_POINT('Ctrl Pts',(-0.238183666596899,-0.0476299999999999,
0.951592097314));
#19780=CARTESIAN_POINT('Ctrl Pts',(-0.233157223576062,-0.0740444353928835,
0.952850216871763));
#19781=CARTESIAN_POINT('Ctrl Pts',(-0.223801617934946,-0.0999305678883309,
0.955173119738174));
#19782=CARTESIAN_POINT('Ctrl Pts',(-0.199966927975188,-0.142345102874864,
0.960411259488514));
#19783=CARTESIAN_POINT('Ctrl Pts',(-0.1868781821531,-0.159766064500479,
0.963103647174702));
#19784=CARTESIAN_POINT('Ctrl Pts',(-0.15681442133453,-0.190326085855194,
0.968453058988463));
#19785=CARTESIAN_POINT('Ctrl Pts',(-0.139836317888043,-0.203463743702801,
0.971100730005489));
#19786=CARTESIAN_POINT('Ctrl Pts',(-0.104422493053067,-0.224161999508995,
0.975530745318961));
#19787=CARTESIAN_POINT('Ctrl Pts',(-0.0842175114474176,-0.232861760990032,
0.977553872336861));
#19788=CARTESIAN_POINT('Ctrl Pts',(-0.0421062857595701,-0.244251601209411,
0.980270995488453));
#19789=CARTESIAN_POINT('Ctrl Pts',(-0.0201990724523197,-0.246942143572133,
0.980948));
#19790=CARTESIAN_POINT('Ctrl Pts',(0.020199072452319,-0.246942143572133,
0.980948));
#19791=CARTESIAN_POINT('Ctrl Pts',(0.0421062857595694,-0.244251601209411,
0.980270995488454));
#19792=CARTESIAN_POINT('Ctrl Pts',(0.0842175114474169,-0.232861760990032,
0.977553872336861));
#19793=CARTESIAN_POINT('Ctrl Pts',(0.104422493053067,-0.224161999508995,
0.975530745318961));
#19794=CARTESIAN_POINT('Ctrl Pts',(0.139836317888042,-0.203463743702801,
0.971100730005489));
#19795=CARTESIAN_POINT('Ctrl Pts',(0.15681442133453,-0.190326085855194,
0.968453058988463));
#19796=CARTESIAN_POINT('Ctrl Pts',(0.1868781821531,-0.15976606450048,0.963103647174702));
#19797=CARTESIAN_POINT('Ctrl Pts',(0.199966927975188,-0.142345102874864,
0.960411259488514));
#19798=CARTESIAN_POINT('Ctrl Pts',(0.223801617934945,-0.0999305678883309,
0.955173119738174));
#19799=CARTESIAN_POINT('Ctrl Pts',(0.233157223576061,-0.0740444353928835,
0.952850216871763));
#19800=CARTESIAN_POINT('Ctrl Pts',(0.238183666596899,-0.0476299999999999,
0.951592097314));
#19801=CARTESIAN_POINT('Origin',(-1.94289029309402E-16,-0.04763,1.));
#19802=CARTESIAN_POINT('Origin',(0.,-0.04763,0.));
#19803=CARTESIAN_POINT('',(-0.504455939115715,-0.04763,0.841298510752802));
#19804=CARTESIAN_POINT('Origin',(0.,-0.04763,0.));
#19805=CARTESIAN_POINT('Origin',(-0.707106781186548,-0.04763,0.707106781186547));
#19806=CARTESIAN_POINT('Origin',(-0.707106781186548,0.,0.707106781186547));
#19807=CARTESIAN_POINT('',(-0.841298510752802,-0.04763,0.504455939115715));
#19808=CARTESIAN_POINT('Ctrl Pts',(-0.841298510752802,-0.04763,0.504455939115715));
#19809=CARTESIAN_POINT('Ctrl Pts',(-0.838633903678357,-0.0740444353928835,
0.508899795931835));
#19810=CARTESIAN_POINT('Ctrl Pts',(-0.833661031856294,-0.0999305678883309,
0.517157748491652));
#19811=CARTESIAN_POINT('Ctrl Pts',(-0.820511285096538,-0.142345102874864,
0.537715343527944));
#19812=CARTESIAN_POINT('Ctrl Pts',(-0.813159949759,-0.159766064500479,0.548874290046456));
#19813=CARTESIAN_POINT('Ctrl Pts',(-0.795684265985089,-0.190326085855194,
0.573915184558107));
#19814=CARTESIAN_POINT('Ctrl Pts',(-0.78555112003688,-0.203463743702801,
0.587792702767295));
#19815=CARTESIAN_POINT('Ctrl Pts',(-0.763642258217233,-0.224161999508995,
0.615966552324775));
#19816=CARTESIAN_POINT('Ctrl Pts',(-0.750785745543687,-0.232861760990032,
0.631684198665438));
#19817=CARTESIAN_POINT('Ctrl Pts',(-0.722929908501543,-0.244251601209411,
0.663382628119203));
#19818=CARTESIAN_POINT('Ctrl Pts',(-0.707917883896095,-0.246942143572133,
0.679352081686668));
#19819=CARTESIAN_POINT('Ctrl Pts',(-0.679352081686668,-0.246942143572133,
0.707917883896095));
#19820=CARTESIAN_POINT('Ctrl Pts',(-0.663382628119203,-0.244251601209411,
0.722929908501544));
#19821=CARTESIAN_POINT('Ctrl Pts',(-0.631684198665438,-0.232861760990031,
0.750785745543687));
#19822=CARTESIAN_POINT('Ctrl Pts',(-0.615966552324775,-0.224161999508995,
0.763642258217233));
#19823=CARTESIAN_POINT('Ctrl Pts',(-0.587792702767295,-0.203463743702801,
0.78555112003688));
#19824=CARTESIAN_POINT('Ctrl Pts',(-0.573915184558107,-0.190326085855194,
0.795684265985088));
#19825=CARTESIAN_POINT('Ctrl Pts',(-0.548874290046456,-0.159766064500479,
0.813159949759));
#19826=CARTESIAN_POINT('Ctrl Pts',(-0.537715343527944,-0.142345102874864,
0.820511285096538));
#19827=CARTESIAN_POINT('Ctrl Pts',(-0.517157748491652,-0.0999305678883309,
0.833661031856294));
#19828=CARTESIAN_POINT('Ctrl Pts',(-0.508899795931835,-0.0740444353928835,
0.838633903678357));
#19829=CARTESIAN_POINT('Ctrl Pts',(-0.504455939115716,-0.04763,0.841298510752801));
#19830=CARTESIAN_POINT('Origin',(-0.707106781186548,-0.04763,0.707106781186547));
#19831=CARTESIAN_POINT('Origin',(0.,-0.04763,0.));
#19832=CARTESIAN_POINT('',(-0.951592097314,-0.04763,0.238183666596899));
#19833=CARTESIAN_POINT('Origin',(0.,-0.04763,0.));
#19834=CARTESIAN_POINT('Origin',(-1.,-0.04763,-1.11022302462516E-16));
#19835=CARTESIAN_POINT('Origin',(-1.,0.,-1.11022302462516E-16));
#19836=CARTESIAN_POINT('',(-0.951592097314,-0.04763,-0.2381836665969));
#19837=CARTESIAN_POINT('',(-0.980948,-0.246942143572133,1.08514323328844E-18));
#19838=CARTESIAN_POINT('Ctrl Pts',(-0.951592097314,-0.04763,-0.238183666596899));
#19839=CARTESIAN_POINT('Ctrl Pts',(-0.952850216871763,-0.0740444353928835,
-0.233157223576062));
#19840=CARTESIAN_POINT('Ctrl Pts',(-0.955173119738174,-0.0999305678883309,
-0.223801617934946));
#19841=CARTESIAN_POINT('Ctrl Pts',(-0.960411259488514,-0.142345102874864,
-0.199966927975188));
#19842=CARTESIAN_POINT('Ctrl Pts',(-0.963103647174702,-0.159766064500479,
-0.1868781821531));
#19843=CARTESIAN_POINT('Ctrl Pts',(-0.968453058988463,-0.190326085855194,
-0.15681442133453));
#19844=CARTESIAN_POINT('Ctrl Pts',(-0.971100730005489,-0.203463743702801,
-0.139836317888043));
#19845=CARTESIAN_POINT('Ctrl Pts',(-0.975530745318961,-0.224161999508995,
-0.104422493053067));
#19846=CARTESIAN_POINT('Ctrl Pts',(-0.977553872336861,-0.232861760990032,
-0.0842175114474175));
#19847=CARTESIAN_POINT('Ctrl Pts',(-0.980270995488453,-0.244251601209411,
-0.0421062857595699));
#19848=CARTESIAN_POINT('Ctrl Pts',(-0.980948,-0.246942143572133,-0.0201990724523195));
#19849=CARTESIAN_POINT('Ctrl Pts',(-0.980948,-0.246942143572133,-1.17961196366423E-16));
#19850=CARTESIAN_POINT('Origin',(-1.,-0.04763,-1.11022302462516E-16));
#19851=CARTESIAN_POINT('Ctrl Pts',(-0.980948,-0.246942143572133,-1.17961196366423E-16));
#19852=CARTESIAN_POINT('Ctrl Pts',(-0.980948,-0.246942143572133,0.0201990724523192));
#19853=CARTESIAN_POINT('Ctrl Pts',(-0.980270995488453,-0.244251601209411,
0.0421062857595695));
#19854=CARTESIAN_POINT('Ctrl Pts',(-0.977553872336861,-0.232861760990032,
0.0842175114474169));
#19855=CARTESIAN_POINT('Ctrl Pts',(-0.975530745318961,-0.224161999508995,
0.104422493053066));
#19856=CARTESIAN_POINT('Ctrl Pts',(-0.971100730005489,-0.203463743702801,
0.139836317888042));
#19857=CARTESIAN_POINT('Ctrl Pts',(-0.968453058988463,-0.190326085855194,
0.15681442133453));
#19858=CARTESIAN_POINT('Ctrl Pts',(-0.963103647174702,-0.15976606450048,
0.1868781821531));
#19859=CARTESIAN_POINT('Ctrl Pts',(-0.960411259488514,-0.142345102874864,
0.199966927975188));
#19860=CARTESIAN_POINT('Ctrl Pts',(-0.955173119738174,-0.099930567888331,
0.223801617934945));
#19861=CARTESIAN_POINT('Ctrl Pts',(-0.952850216871763,-0.0740444353928835,
0.233157223576061));
#19862=CARTESIAN_POINT('Ctrl Pts',(-0.951592097314,-0.04763,0.238183666596899));
#19863=CARTESIAN_POINT('Origin',(0.,-0.04763,0.));
#19864=CARTESIAN_POINT('',(-0.841298510752802,-0.04763,-0.504455939115715));
#19865=CARTESIAN_POINT('Origin',(0.,-0.04763,0.));
#19866=CARTESIAN_POINT('Origin',(-0.707106781186547,-0.04763,-0.707106781186548));
#19867=CARTESIAN_POINT('Origin',(-0.707106781186547,0.,-0.707106781186548));
#19868=CARTESIAN_POINT('',(-0.504455939115715,-0.04763,-0.841298510752802));
#19869=CARTESIAN_POINT('Ctrl Pts',(-0.504455939115715,-0.04763,-0.841298510752802));
#19870=CARTESIAN_POINT('Ctrl Pts',(-0.508899795931835,-0.0740444353928835,
-0.838633903678357));
#19871=CARTESIAN_POINT('Ctrl Pts',(-0.517157748491652,-0.0999305678883309,
-0.833661031856294));
#19872=CARTESIAN_POINT('Ctrl Pts',(-0.537715343527944,-0.142345102874864,
-0.820511285096538));
#19873=CARTESIAN_POINT('Ctrl Pts',(-0.548874290046456,-0.159766064500479,
-0.813159949759));
#19874=CARTESIAN_POINT('Ctrl Pts',(-0.573915184558107,-0.190326085855194,
-0.795684265985089));
#19875=CARTESIAN_POINT('Ctrl Pts',(-0.587792702767295,-0.203463743702801,
-0.78555112003688));
#19876=CARTESIAN_POINT('Ctrl Pts',(-0.615966552324775,-0.224161999508995,
-0.763642258217233));
#19877=CARTESIAN_POINT('Ctrl Pts',(-0.631684198665438,-0.232861760990032,
-0.750785745543687));
#19878=CARTESIAN_POINT('Ctrl Pts',(-0.663382628119203,-0.244251601209411,
-0.722929908501543));
#19879=CARTESIAN_POINT('Ctrl Pts',(-0.679352081686668,-0.246942143572133,
-0.707917883896095));
#19880=CARTESIAN_POINT('Ctrl Pts',(-0.707917883896095,-0.246942143572133,
-0.679352081686668));
#19881=CARTESIAN_POINT('Ctrl Pts',(-0.722929908501543,-0.244251601209411,
-0.663382628119203));
#19882=CARTESIAN_POINT('Ctrl Pts',(-0.750785745543687,-0.232861760990032,
-0.631684198665439));
#19883=CARTESIAN_POINT('Ctrl Pts',(-0.763642258217232,-0.224161999508995,
-0.615966552324775));
#19884=CARTESIAN_POINT('Ctrl Pts',(-0.78555112003688,-0.203463743702801,
-0.587792702767295));
#19885=CARTESIAN_POINT('Ctrl Pts',(-0.795684265985088,-0.190326085855194,
-0.573915184558107));
#19886=CARTESIAN_POINT('Ctrl Pts',(-0.813159949759,-0.15976606450048,-0.548874290046456));
#19887=CARTESIAN_POINT('Ctrl Pts',(-0.820511285096538,-0.142345102874864,
-0.537715343527944));
#19888=CARTESIAN_POINT('Ctrl Pts',(-0.833661031856294,-0.0999305678883311,
-0.517157748491652));
#19889=CARTESIAN_POINT('Ctrl Pts',(-0.838633903678357,-0.0740444353928836,
-0.508899795931835));
#19890=CARTESIAN_POINT('Ctrl Pts',(-0.841298510752801,-0.04763,-0.504455939115715));
#19891=CARTESIAN_POINT('Origin',(-0.707106781186547,-0.04763,-0.707106781186548));
#19892=CARTESIAN_POINT('Origin',(0.,-0.04763,0.));
#19893=CARTESIAN_POINT('',(-0.238183666596899,-0.04763,-0.951592097314));
#19894=CARTESIAN_POINT('Origin',(0.,-0.04763,0.));
#19895=CARTESIAN_POINT('Origin',(5.55111512312578E-17,-0.04763,-1.));
#19896=CARTESIAN_POINT('Origin',(5.55111512312578E-17,0.,-1.));
#19897=CARTESIAN_POINT('',(0.238183666596899,-0.04763,-0.951592097314));
#19898=CARTESIAN_POINT('Ctrl Pts',(0.238183666596899,-0.04763,-0.951592097314));
#19899=CARTESIAN_POINT('Ctrl Pts',(0.233157223576062,-0.0740444353928835,
-0.952850216871763));
#19900=CARTESIAN_POINT('Ctrl Pts',(0.223801617934946,-0.099930567888331,
-0.955173119738174));
#19901=CARTESIAN_POINT('Ctrl Pts',(0.199966927975188,-0.142345102874864,
-0.960411259488514));
#19902=CARTESIAN_POINT('Ctrl Pts',(0.1868781821531,-0.15976606450048,-0.963103647174702));
#19903=CARTESIAN_POINT('Ctrl Pts',(0.15681442133453,-0.190326085855194,
-0.968453058988463));
#19904=CARTESIAN_POINT('Ctrl Pts',(0.139836317888042,-0.203463743702801,
-0.971100730005489));
#19905=CARTESIAN_POINT('Ctrl Pts',(0.104422493053067,-0.224161999508995,
-0.975530745318961));
#19906=CARTESIAN_POINT('Ctrl Pts',(0.0842175114474173,-0.232861760990032,
-0.977553872336861));
#19907=CARTESIAN_POINT('Ctrl Pts',(0.0421062857595698,-0.244251601209411,
-0.980270995488453));
#19908=CARTESIAN_POINT('Ctrl Pts',(0.0201990724523194,-0.246942143572133,
-0.980948));
#19909=CARTESIAN_POINT('Ctrl Pts',(-0.0201990724523193,-0.246942143572133,
-0.980948));
#19910=CARTESIAN_POINT('Ctrl Pts',(-0.0421062857595697,-0.244251601209411,
-0.980270995488453));
#19911=CARTESIAN_POINT('Ctrl Pts',(-0.0842175114474171,-0.232861760990032,
-0.977553872336861));
#19912=CARTESIAN_POINT('Ctrl Pts',(-0.104422493053067,-0.224161999508995,
-0.975530745318961));
#19913=CARTESIAN_POINT('Ctrl Pts',(-0.139836317888042,-0.203463743702801,
-0.971100730005489));
#19914=CARTESIAN_POINT('Ctrl Pts',(-0.15681442133453,-0.190326085855194,
-0.968453058988463));
#19915=CARTESIAN_POINT('Ctrl Pts',(-0.1868781821531,-0.15976606450048,-0.963103647174702));
#19916=CARTESIAN_POINT('Ctrl Pts',(-0.199966927975188,-0.142345102874864,
-0.960411259488514));
#19917=CARTESIAN_POINT('Ctrl Pts',(-0.223801617934945,-0.099930567888331,
-0.955173119738174));
#19918=CARTESIAN_POINT('Ctrl Pts',(-0.233157223576062,-0.0740444353928835,
-0.952850216871763));
#19919=CARTESIAN_POINT('Ctrl Pts',(-0.238183666596899,-0.0476299999999999,
-0.951592097314));
#19920=CARTESIAN_POINT('Origin',(5.55111512312578E-17,-0.04763,-1.));
#19921=CARTESIAN_POINT('Origin',(0.,-0.04763,0.));
#19922=CARTESIAN_POINT('',(0.504455939115715,-0.04763,-0.841298510752802));
#19923=CARTESIAN_POINT('Origin',(0.,-0.04763,0.));
#19924=CARTESIAN_POINT('Origin',(0.707106781186548,-0.04763,-0.707106781186547));
#19925=CARTESIAN_POINT('Origin',(0.707106781186548,0.,-0.707106781186547));
#19926=CARTESIAN_POINT('',(0.841298510752802,-0.04763,-0.504455939115715));
#19927=CARTESIAN_POINT('Ctrl Pts',(0.841298510752802,-0.04763,-0.504455939115715));
#19928=CARTESIAN_POINT('Ctrl Pts',(0.838633903678357,-0.0740444353928835,
-0.508899795931835));
#19929=CARTESIAN_POINT('Ctrl Pts',(0.833661031856294,-0.0999305678883309,
-0.517157748491652));
#19930=CARTESIAN_POINT('Ctrl Pts',(0.820511285096538,-0.142345102874864,
-0.537715343527944));
#19931=CARTESIAN_POINT('Ctrl Pts',(0.813159949759,-0.159766064500479,-0.548874290046456));
#19932=CARTESIAN_POINT('Ctrl Pts',(0.795684265985088,-0.190326085855194,
-0.573915184558107));
#19933=CARTESIAN_POINT('Ctrl Pts',(0.78555112003688,-0.203463743702801,
-0.587792702767295));
#19934=CARTESIAN_POINT('Ctrl Pts',(0.763642258217233,-0.224161999508995,
-0.615966552324775));
#19935=CARTESIAN_POINT('Ctrl Pts',(0.750785745543687,-0.232861760990032,
-0.631684198665438));
#19936=CARTESIAN_POINT('Ctrl Pts',(0.722929908501543,-0.244251601209411,
-0.663382628119203));
#19937=CARTESIAN_POINT('Ctrl Pts',(0.707917883896095,-0.246942143572133,
-0.679352081686668));
#19938=CARTESIAN_POINT('Ctrl Pts',(0.679352081686668,-0.246942143572133,
-0.707917883896095));
#19939=CARTESIAN_POINT('Ctrl Pts',(0.663382628119203,-0.244251601209411,
-0.722929908501543));
#19940=CARTESIAN_POINT('Ctrl Pts',(0.631684198665438,-0.232861760990032,
-0.750785745543687));
#19941=CARTESIAN_POINT('Ctrl Pts',(0.615966552324775,-0.224161999508995,
-0.763642258217232));
#19942=CARTESIAN_POINT('Ctrl Pts',(0.587792702767295,-0.203463743702801,
-0.78555112003688));
#19943=CARTESIAN_POINT('Ctrl Pts',(0.573915184558107,-0.190326085855194,
-0.795684265985088));
#19944=CARTESIAN_POINT('Ctrl Pts',(0.548874290046456,-0.159766064500479,
-0.813159949759));
#19945=CARTESIAN_POINT('Ctrl Pts',(0.537715343527944,-0.142345102874864,
-0.820511285096538));
#19946=CARTESIAN_POINT('Ctrl Pts',(0.517157748491652,-0.099930567888331,
-0.833661031856294));
#19947=CARTESIAN_POINT('Ctrl Pts',(0.508899795931835,-0.0740444353928835,
-0.838633903678357));
#19948=CARTESIAN_POINT('Ctrl Pts',(0.504455939115715,-0.04763,-0.841298510752801));
#19949=CARTESIAN_POINT('Origin',(0.707106781186548,-0.04763,-0.707106781186547));
#19950=CARTESIAN_POINT('Origin',(0.,-0.166705,0.));
#19951=CARTESIAN_POINT('',(-0.980948,-0.28578,1.20131482833E-16));
#19952=CARTESIAN_POINT('Origin',(0.,-0.28578,0.));
#19953=CARTESIAN_POINT('',(-0.980948,-0.166705,1.20131482833E-16));
#19954=CARTESIAN_POINT('',(0.951592097314,-0.04763,0.238183666596899));
#19955=CARTESIAN_POINT('Origin',(0.,-0.04763,0.));
#19956=CARTESIAN_POINT('',(0.951592097314,-0.04763,-0.238183666596899));
#19957=CARTESIAN_POINT('Ctrl Pts',(0.951592097314,-0.04763,0.238183666596899));
#19958=CARTESIAN_POINT('Ctrl Pts',(0.952850216871763,-0.0740444353928835,
0.233157223576062));
#19959=CARTESIAN_POINT('Ctrl Pts',(0.955173119738174,-0.099930567888331,
0.223801617934945));
#19960=CARTESIAN_POINT('Ctrl Pts',(0.960411259488514,-0.142345102874864,
0.199966927975188));
#19961=CARTESIAN_POINT('Ctrl Pts',(0.963103647174702,-0.15976606450048,
0.1868781821531));
#19962=CARTESIAN_POINT('Ctrl Pts',(0.968453058988463,-0.190326085855194,
0.15681442133453));
#19963=CARTESIAN_POINT('Ctrl Pts',(0.971100730005489,-0.203463743702801,
0.139836317888042));
#19964=CARTESIAN_POINT('Ctrl Pts',(0.975530745318961,-0.224161999508995,
0.104422493053067));
#19965=CARTESIAN_POINT('Ctrl Pts',(0.977553872336861,-0.232861760990032,
0.0842175114474172));
#19966=CARTESIAN_POINT('Ctrl Pts',(0.980270995488453,-0.244251601209411,
0.0421062857595697));
#19967=CARTESIAN_POINT('Ctrl Pts',(0.980948,-0.246942143572133,0.0201990724523194));
#19968=CARTESIAN_POINT('Ctrl Pts',(0.980948,-0.246942143572133,-0.0201990724523194));
#19969=CARTESIAN_POINT('Ctrl Pts',(0.980270995488453,-0.244251601209411,
-0.0421062857595697));
#19970=CARTESIAN_POINT('Ctrl Pts',(0.977553872336861,-0.232861760990032,
-0.0842175114474172));
#19971=CARTESIAN_POINT('Ctrl Pts',(0.975530745318961,-0.224161999508995,
-0.104422493053067));
#19972=CARTESIAN_POINT('Ctrl Pts',(0.971100730005489,-0.203463743702801,
-0.139836317888042));
#19973=CARTESIAN_POINT('Ctrl Pts',(0.968453058988463,-0.190326085855194,
-0.15681442133453));
#19974=CARTESIAN_POINT('Ctrl Pts',(0.963103647174702,-0.15976606450048,
-0.1868781821531));
#19975=CARTESIAN_POINT('Ctrl Pts',(0.960411259488514,-0.142345102874864,
-0.199966927975188));
#19976=CARTESIAN_POINT('Ctrl Pts',(0.955173119738174,-0.099930567888331,
-0.223801617934945));
#19977=CARTESIAN_POINT('Ctrl Pts',(0.952850216871763,-0.0740444353928835,
-0.233157223576062));
#19978=CARTESIAN_POINT('Ctrl Pts',(0.951592097314,-0.0476299999999999,-0.238183666596899));
#19979=CARTESIAN_POINT('Origin',(0.,-0.04763,0.));
#19980=CARTESIAN_POINT('Origin',(0.,-0.04763,0.));
#19981=CARTESIAN_POINT('Origin',(1.,-0.04763,0.));
#19982=CARTESIAN_POINT('Origin',(1.,0.,0.));
#19983=CARTESIAN_POINT('Origin',(1.,-0.04763,0.));
#19984=CARTESIAN_POINT('Origin',(0.,-0.28578,0.));
#19985=CARTESIAN_POINT('Origin',(0.,-0.04763,0.));
#19986=CARTESIAN_POINT('',(0.,0.,0.));
#19987=CARTESIAN_POINT('Origin',(1.013815,0.445,0.));
#19988=CARTESIAN_POINT('',(-1.013815,0.445,-1.24156529467757E-16));
#19989=CARTESIAN_POINT('Origin',(0.,0.445,0.));
#19990=CARTESIAN_POINT('',(-0.991185,0.445,-1.21385153761287E-16));
#19991=CARTESIAN_POINT('Origin',(0.,0.445,0.));
#19992=CARTESIAN_POINT('Origin',(0.,0.4075,0.));
#19993=CARTESIAN_POINT('',(-1.013815,0.37,-1.24156529467757E-16));
#19994=CARTESIAN_POINT('Origin',(0.,0.37,0.));
#19995=CARTESIAN_POINT('',(-1.013815,0.4075,-1.24156529467757E-16));
#19996=CARTESIAN_POINT('Origin',(0.991185,0.37,0.));
#19997=CARTESIAN_POINT('',(-0.991185,0.37,-1.21385153761287E-16));
#19998=CARTESIAN_POINT('Origin',(0.,0.37,0.));
#19999=CARTESIAN_POINT('Origin',(0.,0.4075,0.));
#20000=CARTESIAN_POINT('',(-0.991185,0.4075,-1.21385153761287E-16));
#20001=CARTESIAN_POINT('Origin',(1.013815,-0.37,0.));
#20002=CARTESIAN_POINT('',(-1.013815,-0.37,-1.24156529467757E-16));
#20003=CARTESIAN_POINT('Origin',(0.,-0.37,0.));
#20004=CARTESIAN_POINT('',(-0.991185,-0.37,-1.21385153761287E-16));
#20005=CARTESIAN_POINT('Origin',(0.,-0.37,0.));
#20006=CARTESIAN_POINT('Origin',(0.,-0.4075,0.));
#20007=CARTESIAN_POINT('',(-1.013815,-0.445,-1.24156529467757E-16));
#20008=CARTESIAN_POINT('Origin',(0.,-0.445,0.));
#20009=CARTESIAN_POINT('',(-1.013815,-0.4075,-1.24156529467757E-16));
#20010=CARTESIAN_POINT('Origin',(0.991185,-0.445,0.));
#20011=CARTESIAN_POINT('',(-0.991185,-0.445,-1.21385153761287E-16));
#20012=CARTESIAN_POINT('Origin',(0.,-0.445,0.));
#20013=CARTESIAN_POINT('Origin',(0.,-0.4075,0.));
#20014=CARTESIAN_POINT('',(-0.991185,-0.4075,-1.21385153761287E-16));
#20015=CARTESIAN_POINT('',(0.,0.,0.));
#20016=CARTESIAN_POINT('',(0.,0.,0.));
#20017=CARTESIAN_POINT('',(0.,0.,0.));
#20018=CARTESIAN_POINT('',(0.,0.,0.));
#20019=CARTESIAN_POINT('',(0.,0.,0.));
#20020=CARTESIAN_POINT('',(0.,0.,0.));
#20021=CARTESIAN_POINT('',(0.,0.,0.));
#20022=CARTESIAN_POINT('Origin',(12.5,11.7,2.3));
#20023=CARTESIAN_POINT('',(12.275,11.7,2.4));
#20024=CARTESIAN_POINT('Origin',(12.5,11.7,2.4));
#20025=CARTESIAN_POINT('',(12.275,11.7,3.2));
#20026=CARTESIAN_POINT('',(12.275,11.7,2.3));
#20027=CARTESIAN_POINT('Origin',(12.5,11.7,3.2));
#20028=CARTESIAN_POINT('Origin',(11.5,10.3,2.3));
#20029=CARTESIAN_POINT('',(11.275,10.3,2.4));
#20030=CARTESIAN_POINT('Origin',(11.5,10.3,2.4));
#20031=CARTESIAN_POINT('',(11.275,10.3,3.2));
#20032=CARTESIAN_POINT('',(11.275,10.3,2.3));
#20033=CARTESIAN_POINT('Origin',(11.5,10.3,3.2));
#20034=CARTESIAN_POINT('Origin',(12.8,-1.,2.3));
#20035=CARTESIAN_POINT('',(12.635,-1.,2.4));
#20036=CARTESIAN_POINT('Origin',(12.8,-1.,2.4));
#20037=CARTESIAN_POINT('',(12.635,-1.,3.2));
#20038=CARTESIAN_POINT('',(12.635,-1.,2.3));
#20039=CARTESIAN_POINT('Origin',(12.8,-1.,3.2));
#20040=CARTESIAN_POINT('Origin',(7.2,1.,2.3));
#20041=CARTESIAN_POINT('',(7.035,1.,2.4));
#20042=CARTESIAN_POINT('Origin',(7.2,1.,2.4));
#20043=CARTESIAN_POINT('',(7.035,1.,3.2));
#20044=CARTESIAN_POINT('',(7.035,1.,2.3));
#20045=CARTESIAN_POINT('Origin',(7.2,1.,3.2));
#20046=CARTESIAN_POINT('Origin',(7.2,-1.,2.3));
#20047=CARTESIAN_POINT('',(7.035,-1.,2.4));
#20048=CARTESIAN_POINT('Origin',(7.2,-1.,2.4));
#20049=CARTESIAN_POINT('',(7.035,-1.,3.2));
#20050=CARTESIAN_POINT('',(7.035,-1.,2.3));
#20051=CARTESIAN_POINT('Origin',(7.2,-1.,3.2));
#20052=CARTESIAN_POINT('Origin',(12.8,1.,2.3));
#20053=CARTESIAN_POINT('',(12.635,1.,2.4));
#20054=CARTESIAN_POINT('Origin',(12.8,1.,2.4));
#20055=CARTESIAN_POINT('',(12.635,1.,3.2));
#20056=CARTESIAN_POINT('',(12.635,1.,2.3));
#20057=CARTESIAN_POINT('Origin',(12.8,1.,3.2));
#20058=CARTESIAN_POINT('Origin',(11.5,-1.9,2.3));
#20059=CARTESIAN_POINT('',(11.225,-1.9,2.4));
#20060=CARTESIAN_POINT('Origin',(11.5,-1.9,2.4));
#20061=CARTESIAN_POINT('',(11.225,-1.9,3.2));
#20062=CARTESIAN_POINT('',(11.225,-1.9,2.3));
#20063=CARTESIAN_POINT('Origin',(11.5,-1.9,3.2));
#20064=CARTESIAN_POINT('Origin',(8.5,1.9,2.3));
#20065=CARTESIAN_POINT('',(8.225,1.9,2.4));
#20066=CARTESIAN_POINT('Origin',(8.5,1.9,2.4));
#20067=CARTESIAN_POINT('',(8.225,1.9,3.2));
#20068=CARTESIAN_POINT('',(8.225,1.9,2.3));
#20069=CARTESIAN_POINT('Origin',(8.5,1.9,3.2));
#20070=CARTESIAN_POINT('Origin',(8.5,-1.9,2.3));
#20071=CARTESIAN_POINT('',(8.225,-1.9,2.4));
#20072=CARTESIAN_POINT('Origin',(8.5,-1.9,2.4));
#20073=CARTESIAN_POINT('',(8.225,-1.9,3.2));
#20074=CARTESIAN_POINT('',(8.225,-1.9,2.3));
#20075=CARTESIAN_POINT('Origin',(8.5,-1.9,3.2));
#20076=CARTESIAN_POINT('Origin',(11.5,1.9,2.3));
#20077=CARTESIAN_POINT('',(11.225,1.9,2.4));
#20078=CARTESIAN_POINT('Origin',(11.5,1.9,2.4));
#20079=CARTESIAN_POINT('',(11.225,1.9,3.2));
#20080=CARTESIAN_POINT('',(11.225,1.9,2.3));
#20081=CARTESIAN_POINT('Origin',(11.5,1.9,3.2));
#20082=CARTESIAN_POINT('Origin',(14.,12.5,2.4));
#20083=CARTESIAN_POINT('',(14.,12.5,2.4));
#20084=CARTESIAN_POINT('',(6.5,12.5,2.4));
#20085=CARTESIAN_POINT('',(14.,12.5,2.4));
#20086=CARTESIAN_POINT('',(6.5,12.5,3.2));
#20087=CARTESIAN_POINT('',(6.5,12.5,2.4));
#20088=CARTESIAN_POINT('',(14.,12.5,3.2));
#20089=CARTESIAN_POINT('',(14.,12.5,3.2));
#20090=CARTESIAN_POINT('',(14.,12.5,2.4));
#20091=CARTESIAN_POINT('Origin',(14.,-2.5,2.4));
#20092=CARTESIAN_POINT('',(14.,-2.5,2.4));
#20093=CARTESIAN_POINT('',(14.,-2.5,2.4));
#20094=CARTESIAN_POINT('',(14.,-2.5,3.2));
#20095=CARTESIAN_POINT('',(14.,-2.5,3.2));
#20096=CARTESIAN_POINT('',(14.,-2.5,2.4));
#20097=CARTESIAN_POINT('Origin',(6.5,-2.5,2.4));
#20098=CARTESIAN_POINT('',(6.5,-2.5,2.4));
#20099=CARTESIAN_POINT('',(6.5,-2.5,2.4));
#20100=CARTESIAN_POINT('',(6.5,-2.5,3.2));
#20101=CARTESIAN_POINT('',(6.5,-2.5,3.2));
#20102=CARTESIAN_POINT('',(6.5,-2.5,2.4));
#20103=CARTESIAN_POINT('Origin',(6.5,12.5,2.4));
#20104=CARTESIAN_POINT('',(6.5,12.5,2.4));
#20105=CARTESIAN_POINT('',(6.5,12.5,3.2));
#20106=CARTESIAN_POINT('Origin',(10.25,5.,3.2));
#20107=CARTESIAN_POINT('Origin',(10.25,5.,2.4));
#20108=CARTESIAN_POINT('',(0.,0.,0.));
#20109=CARTESIAN_POINT('Origin',(8.5857864376269,-1.9,5.58578643762691));
#20110=CARTESIAN_POINT('',(8.42078643762691,-1.8,5.58578643762691));
#20111=CARTESIAN_POINT('Origin',(8.5857864376269,-1.8,5.58578643762691));
#20112=CARTESIAN_POINT('',(8.42078643762691,1.8,5.58578643762691));
#20113=CARTESIAN_POINT('',(8.42078643762691,-1.9,5.58578643762691));
#20114=CARTESIAN_POINT('Origin',(8.5857864376269,1.8,5.58578643762691));
#20115=CARTESIAN_POINT('Origin',(8.5857864376269,-1.9,8.4142135623731));
#20116=CARTESIAN_POINT('',(8.42078643762691,-1.8,8.4142135623731));
#20117=CARTESIAN_POINT('Origin',(8.5857864376269,-1.8,8.4142135623731));
#20118=CARTESIAN_POINT('',(8.42078643762691,1.8,8.4142135623731));
#20119=CARTESIAN_POINT('',(8.42078643762691,-1.9,8.4142135623731));
#20120=CARTESIAN_POINT('Origin',(8.5857864376269,1.8,8.4142135623731));
#20121=CARTESIAN_POINT('Origin',(11.4142135623731,-1.9,8.4142135623731));
#20122=CARTESIAN_POINT('',(11.2492135623731,-1.8,8.4142135623731));
#20123=CARTESIAN_POINT('Origin',(11.4142135623731,-1.8,8.4142135623731));
#20124=CARTESIAN_POINT('',(11.2492135623731,1.8,8.4142135623731));
#20125=CARTESIAN_POINT('',(11.2492135623731,-1.9,8.4142135623731));
#20126=CARTESIAN_POINT('Origin',(11.4142135623731,1.8,8.4142135623731));
#20127=CARTESIAN_POINT('Origin',(11.4142135623731,-1.9,5.58578643762691));
#20128=CARTESIAN_POINT('',(11.2492135623731,-1.8,5.58578643762691));
#20129=CARTESIAN_POINT('Origin',(11.4142135623731,-1.8,5.58578643762691));
#20130=CARTESIAN_POINT('',(11.2492135623731,1.8,5.58578643762691));
#20131=CARTESIAN_POINT('',(11.2492135623731,-1.9,5.58578643762691));
#20132=CARTESIAN_POINT('Origin',(11.4142135623731,1.8,5.58578643762691));
#20133=CARTESIAN_POINT('Origin',(10.,-1.9,7.));
#20134=CARTESIAN_POINT('',(8.4,-1.8,7.));
#20135=CARTESIAN_POINT('Origin',(10.,-1.8,7.));
#20136=CARTESIAN_POINT('',(8.4,1.8,7.));
#20137=CARTESIAN_POINT('',(8.4,-1.9,7.));
#20138=CARTESIAN_POINT('Origin',(10.,1.8,7.));
#20139=CARTESIAN_POINT('Origin',(11.5,-1.9,3.8));
#20140=CARTESIAN_POINT('',(10.9846117967978,-1.8,3.8));
#20141=CARTESIAN_POINT('',(12.0153882032022,-1.8,3.8));
#20142=CARTESIAN_POINT('',(9.65,-1.8,3.8));
#20143=CARTESIAN_POINT('Origin',(11.5,-1.9,3.8));
#20144=CARTESIAN_POINT('Origin',(11.5,-1.9,3.1));
#20145=CARTESIAN_POINT('',(10.9846117967978,-1.8,3.2));
#20146=CARTESIAN_POINT('',(10.9846117967978,-1.8,3.1));
#20147=CARTESIAN_POINT('',(12.0153882032022,-1.8,3.2));
#20148=CARTESIAN_POINT('Origin',(11.5,-1.9,3.2));
#20149=CARTESIAN_POINT('',(12.0153882032022,-1.8,3.1));
#20150=CARTESIAN_POINT('Origin',(8.5,1.9,3.8));
#20151=CARTESIAN_POINT('',(9.01538820320221,1.8,3.8));
#20152=CARTESIAN_POINT('',(7.98461179679779,1.8,3.8));
#20153=CARTESIAN_POINT('',(10.35,1.8,3.8));
#20154=CARTESIAN_POINT('Origin',(8.5,1.9,3.8));
#20155=CARTESIAN_POINT('Origin',(8.5,1.9,3.1));
#20156=CARTESIAN_POINT('',(9.01538820320221,1.8,3.2));
#20157=CARTESIAN_POINT('',(9.01538820320221,1.8,3.1));
#20158=CARTESIAN_POINT('',(7.98461179679779,1.8,3.2));
#20159=CARTESIAN_POINT('Origin',(8.5,1.9,3.2));
#20160=CARTESIAN_POINT('',(7.98461179679779,1.8,3.1));
#20161=CARTESIAN_POINT('Origin',(8.5,-1.9,3.8));
#20162=CARTESIAN_POINT('',(7.98461179679779,-1.8,3.8));
#20163=CARTESIAN_POINT('',(9.01538820320221,-1.8,3.8));
#20164=CARTESIAN_POINT('',(8.15,-1.8,3.8));
#20165=CARTESIAN_POINT('Origin',(8.5,-1.9,3.8));
#20166=CARTESIAN_POINT('Origin',(8.5,-1.9,3.1));
#20167=CARTESIAN_POINT('',(7.98461179679779,-1.8,3.2));
#20168=CARTESIAN_POINT('',(7.98461179679779,-1.8,3.1));
#20169=CARTESIAN_POINT('',(9.01538820320221,-1.8,3.2));
#20170=CARTESIAN_POINT('Origin',(8.5,-1.9,3.2));
#20171=CARTESIAN_POINT('',(9.01538820320221,-1.8,3.1));
#20172=CARTESIAN_POINT('Origin',(11.5,1.9,3.8));
#20173=CARTESIAN_POINT('',(12.0153882032022,1.8,3.8));
#20174=CARTESIAN_POINT('',(10.9846117967978,1.8,3.8));
#20175=CARTESIAN_POINT('',(11.85,1.8,3.8));
#20176=CARTESIAN_POINT('Origin',(11.5,1.9,3.8));
#20177=CARTESIAN_POINT('Origin',(11.5,1.9,3.1));
#20178=CARTESIAN_POINT('',(12.0153882032022,1.8,3.2));
#20179=CARTESIAN_POINT('',(12.0153882032022,1.8,3.1));
#20180=CARTESIAN_POINT('',(10.9846117967978,1.8,3.2));
#20181=CARTESIAN_POINT('Origin',(11.5,1.9,3.2));
#20182=CARTESIAN_POINT('',(10.9846117967978,1.8,3.1));
#20183=CARTESIAN_POINT('Origin',(7.8,-1.8,3.2));
#20184=CARTESIAN_POINT('',(13.4,-1.8,3.2));
#20185=CARTESIAN_POINT('',(6.6,-1.8,3.2));
#20186=CARTESIAN_POINT('',(13.4,-1.8,4.));
#20187=CARTESIAN_POINT('',(13.4,-1.8,3.2));
#20188=CARTESIAN_POINT('',(12.2,-1.8,4.));
#20189=CARTESIAN_POINT('',(13.4,-1.8,4.));
#20190=CARTESIAN_POINT('',(12.2,-1.8,9.2));
#20191=CARTESIAN_POINT('',(12.2,-1.8,3.2));
#20192=CARTESIAN_POINT('',(7.8,-1.8,9.2));
#20193=CARTESIAN_POINT('',(7.8,-1.8,9.2));
#20194=CARTESIAN_POINT('',(7.8,-1.8,4.));
#20195=CARTESIAN_POINT('',(7.8,-1.8,3.2));
#20196=CARTESIAN_POINT('',(6.6,-1.8,4.));
#20197=CARTESIAN_POINT('',(13.4,-1.8,4.));
#20198=CARTESIAN_POINT('',(6.6,-1.8,3.2));
#20199=CARTESIAN_POINT('',(6.6,-1.8,4.));
#20200=CARTESIAN_POINT('',(6.6,-1.8,3.2));
#20201=CARTESIAN_POINT('',(6.6,-1.8,3.2));
#20202=CARTESIAN_POINT('Origin',(12.2,1.8,3.2));
#20203=CARTESIAN_POINT('',(6.6,1.8,3.2));
#20204=CARTESIAN_POINT('',(6.6,1.8,3.2));
#20205=CARTESIAN_POINT('',(6.6,1.8,4.));
#20206=CARTESIAN_POINT('',(6.6,1.8,4.));
#20207=CARTESIAN_POINT('',(7.8,1.8,4.));
#20208=CARTESIAN_POINT('',(13.4,1.8,4.));
#20209=CARTESIAN_POINT('',(7.8,1.8,9.2));
#20210=CARTESIAN_POINT('',(7.8,1.8,3.2));
#20211=CARTESIAN_POINT('',(12.2,1.8,9.2));
#20212=CARTESIAN_POINT('',(12.2,1.8,9.2));
#20213=CARTESIAN_POINT('',(12.2,1.8,4.));
#20214=CARTESIAN_POINT('',(12.2,1.8,3.2));
#20215=CARTESIAN_POINT('',(13.4,1.8,4.));
#20216=CARTESIAN_POINT('',(13.4,1.8,4.));
#20217=CARTESIAN_POINT('',(13.4,1.8,3.2));
#20218=CARTESIAN_POINT('',(13.4,1.8,3.2));
#20219=CARTESIAN_POINT('',(6.6,1.8,3.2));
#20220=CARTESIAN_POINT('',(6.6,1.8,3.2));
#20221=CARTESIAN_POINT('Origin',(12.8,-1.,3.1));
#20222=CARTESIAN_POINT('',(12.575,-1.,3.2));
#20223=CARTESIAN_POINT('Origin',(12.8,-1.,3.2));
#20224=CARTESIAN_POINT('',(12.575,-1.,4.));
#20225=CARTESIAN_POINT('',(12.575,-1.,3.1));
#20226=CARTESIAN_POINT('Origin',(12.8,-1.,4.));
#20227=CARTESIAN_POINT('Origin',(7.2,1.,3.1));
#20228=CARTESIAN_POINT('',(6.975,1.,3.2));
#20229=CARTESIAN_POINT('Origin',(7.2,1.,3.2));
#20230=CARTESIAN_POINT('',(6.975,1.,4.));
#20231=CARTESIAN_POINT('',(6.975,1.,3.1));
#20232=CARTESIAN_POINT('Origin',(7.2,1.,4.));
#20233=CARTESIAN_POINT('Origin',(7.2,-1.,3.1));
#20234=CARTESIAN_POINT('',(6.975,-1.,3.2));
#20235=CARTESIAN_POINT('Origin',(7.2,-1.,3.2));
#20236=CARTESIAN_POINT('',(6.975,-1.,4.));
#20237=CARTESIAN_POINT('',(6.975,-1.,3.1));
#20238=CARTESIAN_POINT('Origin',(7.2,-1.,4.));
#20239=CARTESIAN_POINT('Origin',(12.8,1.,3.1));
#20240=CARTESIAN_POINT('',(12.575,1.,3.2));
#20241=CARTESIAN_POINT('Origin',(12.8,1.,3.2));
#20242=CARTESIAN_POINT('',(12.575,1.,4.));
#20243=CARTESIAN_POINT('',(12.575,1.,3.1));
#20244=CARTESIAN_POINT('Origin',(12.8,1.,4.));
#20245=CARTESIAN_POINT('Origin',(6.6,-1.8,4.));
#20246=CARTESIAN_POINT('',(12.2,-1.8,4.));
#20247=CARTESIAN_POINT('',(13.4,-1.8,4.));
#20248=CARTESIAN_POINT('Origin',(6.6,-1.8,4.));
#20249=CARTESIAN_POINT('',(7.8,0.,4.));
#20250=CARTESIAN_POINT('',(6.6,-1.8,4.));
#20251=CARTESIAN_POINT('Origin',(6.6,-1.8,3.2));
#20252=CARTESIAN_POINT('',(6.6,-1.8,3.2));
#20253=CARTESIAN_POINT('Origin',(13.4,-1.8,4.));
#20254=CARTESIAN_POINT('',(13.4,-1.8,3.2));
#20255=CARTESIAN_POINT('Origin',(12.2,-1.8,3.2));
#20256=CARTESIAN_POINT('',(12.2,-1.8,9.2));
#20257=CARTESIAN_POINT('Origin',(7.8,1.8,3.2));
#20258=CARTESIAN_POINT('',(7.8,1.8,9.2));
#20259=CARTESIAN_POINT('Origin',(10.,0.,9.2));
#20260=CARTESIAN_POINT('Origin',(10.,0.,3.2));
#20261=CARTESIAN_POINT('',(0.,0.,0.));
#20262=CARTESIAN_POINT('Origin',(10.,-0.4,7.));
#20263=CARTESIAN_POINT('',(8.8,0.4,7.));
#20264=CARTESIAN_POINT('Origin',(10.,0.4,7.));
#20265=CARTESIAN_POINT('',(8.8,-0.4,7.));
#20266=CARTESIAN_POINT('',(8.8,-0.4,7.));
#20267=CARTESIAN_POINT('Origin',(10.,-0.4,7.));
#20268=CARTESIAN_POINT('Origin',(10.,-0.4,7.));
#20269=CARTESIAN_POINT('',(8.41,0.4,7.));
#20270=CARTESIAN_POINT('Origin',(10.,0.4,7.));
#20271=CARTESIAN_POINT('',(8.41,-0.4,7.));
#20272=CARTESIAN_POINT('',(8.41,-0.4,7.));
#20273=CARTESIAN_POINT('Origin',(10.,-0.4,7.));
#20274=CARTESIAN_POINT('Origin',(10.,0.4,7.));
#20275=CARTESIAN_POINT('Origin',(10.,-0.4,7.));
#20276=CARTESIAN_POINT('',(0.,0.,0.));
#20277=CARTESIAN_POINT('Origin',(8.5857864376269,-2.2,5.58578643762691));
#20278=CARTESIAN_POINT('',(8.52266468006184,-2.1,5.3698219874924));
#20279=CARTESIAN_POINT('',(8.52266468006184,-1.8,5.3698219874924));
#20280=CARTESIAN_POINT('',(8.52266468006184,-2.2,5.3698219874924));
#20281=CARTESIAN_POINT('',(8.3698219874924,-2.1,5.52266468006184));
#20282=CARTESIAN_POINT('Origin',(8.5857864376269,-2.1,5.58578643762691));
#20283=CARTESIAN_POINT('',(8.3698219874924,-1.8,5.52266468006184));
#20284=CARTESIAN_POINT('',(8.3698219874924,-2.2,5.52266468006184));
#20285=CARTESIAN_POINT('Origin',(8.5857864376269,-1.8,5.58578643762691));
#20286=CARTESIAN_POINT('Origin',(8.5857864376269,-2.2,8.4142135623731));
#20287=CARTESIAN_POINT('',(8.3698219874924,-2.1,8.47733531993816));
#20288=CARTESIAN_POINT('',(8.3698219874924,-1.8,8.47733531993816));
#20289=CARTESIAN_POINT('',(8.3698219874924,-2.2,8.47733531993816));
#20290=CARTESIAN_POINT('',(8.52266468006184,-2.1,8.6301780125076));
#20291=CARTESIAN_POINT('Origin',(8.5857864376269,-2.1,8.4142135623731));
#20292=CARTESIAN_POINT('',(8.52266468006184,-1.8,8.6301780125076));
#20293=CARTESIAN_POINT('',(8.52266468006184,-2.2,8.6301780125076));
#20294=CARTESIAN_POINT('Origin',(8.5857864376269,-1.8,8.4142135623731));
#20295=CARTESIAN_POINT('Origin',(11.4142135623731,-2.2,8.4142135623731));
#20296=CARTESIAN_POINT('',(11.4773353199382,-2.1,8.6301780125076));
#20297=CARTESIAN_POINT('',(11.4773353199382,-1.8,8.6301780125076));
#20298=CARTESIAN_POINT('',(11.4773353199382,-2.2,8.6301780125076));
#20299=CARTESIAN_POINT('',(11.6301780125076,-2.1,8.47733531993816));
#20300=CARTESIAN_POINT('Origin',(11.4142135623731,-2.1,8.4142135623731));
#20301=CARTESIAN_POINT('',(11.6301780125076,-1.8,8.47733531993816));
#20302=CARTESIAN_POINT('',(11.6301780125076,-2.2,8.47733531993816));
#20303=CARTESIAN_POINT('Origin',(11.4142135623731,-1.8,8.4142135623731));
#20304=CARTESIAN_POINT('Origin',(11.4142135623731,-2.2,5.58578643762691));
#20305=CARTESIAN_POINT('',(11.6301780125076,-2.1,5.52266468006184));
#20306=CARTESIAN_POINT('',(11.6301780125076,-1.8,5.52266468006184));
#20307=CARTESIAN_POINT('',(11.6301780125076,-2.2,5.52266468006184));
#20308=CARTESIAN_POINT('',(11.4773353199382,-2.1,5.3698219874924));
#20309=CARTESIAN_POINT('Origin',(11.4142135623731,-2.1,5.58578643762691));
#20310=CARTESIAN_POINT('',(11.4773353199382,-1.8,5.3698219874924));
#20311=CARTESIAN_POINT('',(11.4773353199382,-2.2,5.3698219874924));
#20312=CARTESIAN_POINT('Origin',(11.4142135623731,-1.8,5.58578643762691));
#20313=CARTESIAN_POINT('Origin',(10.,-2.1,7.));
#20314=CARTESIAN_POINT('Origin',(10.,-2.1,7.));
#20315=CARTESIAN_POINT('Origin',(10.,-2.1,7.));
#20316=CARTESIAN_POINT('Origin',(10.,-2.1,7.));
#20317=CARTESIAN_POINT('Origin',(10.,-2.1,7.));
#20318=CARTESIAN_POINT('',(8.8,-2.1,7.));
#20319=CARTESIAN_POINT('Origin',(10.,-2.1,7.));
#20320=CARTESIAN_POINT('Origin',(10.,-2.1,7.));
#20321=CARTESIAN_POINT('Origin',(10.,-1.8,7.));
#20322=CARTESIAN_POINT('Origin',(10.,-2.1,7.));
#20323=CARTESIAN_POINT('Origin',(10.,-1.8,7.));
#20324=CARTESIAN_POINT('Origin',(10.,-2.1,7.));
#20325=CARTESIAN_POINT('Origin',(10.,-1.8,7.));
#20326=CARTESIAN_POINT('Origin',(10.,-2.1,7.));
#20327=CARTESIAN_POINT('Origin',(10.,-1.8,7.));
#20328=CARTESIAN_POINT('Origin',(10.,-1.8,7.));
#20329=CARTESIAN_POINT('',(8.41,-1.4,7.));
#20330=CARTESIAN_POINT('Origin',(10.,-1.4,7.));
#20331=CARTESIAN_POINT('',(8.41,-1.8,7.));
#20332=CARTESIAN_POINT('',(8.41,-1.8,7.));
#20333=CARTESIAN_POINT('Origin',(10.,-1.8,7.));
#20334=CARTESIAN_POINT('Origin',(10.,-1.4,7.));
#20335=CARTESIAN_POINT('',(8.8,-1.4,7.));
#20336=CARTESIAN_POINT('Origin',(10.,-1.4,7.));
#20337=CARTESIAN_POINT('Origin',(10.,-2.1,7.));
#20338=CARTESIAN_POINT('',(8.8,-2.1,7.));
#20339=CARTESIAN_POINT('Origin',(10.,-1.8,7.));
#20340=CARTESIAN_POINT('',(0.,0.,0.));
#20341=CARTESIAN_POINT('Origin',(8.5857864376269,1.7,5.58578643762691));
#20342=CARTESIAN_POINT('',(8.52266468006184,1.8,5.3698219874924));
#20343=CARTESIAN_POINT('',(8.52266468006184,2.1,5.3698219874924));
#20344=CARTESIAN_POINT('',(8.52266468006184,1.7,5.3698219874924));
#20345=CARTESIAN_POINT('',(8.3698219874924,1.8,5.52266468006184));
#20346=CARTESIAN_POINT('Origin',(8.5857864376269,1.8,5.58578643762691));
#20347=CARTESIAN_POINT('',(8.3698219874924,2.1,5.52266468006184));
#20348=CARTESIAN_POINT('',(8.3698219874924,1.7,5.52266468006184));
#20349=CARTESIAN_POINT('Origin',(8.5857864376269,2.1,5.58578643762691));
#20350=CARTESIAN_POINT('Origin',(8.5857864376269,1.7,8.4142135623731));
#20351=CARTESIAN_POINT('',(8.3698219874924,1.8,8.47733531993816));
#20352=CARTESIAN_POINT('',(8.3698219874924,2.1,8.47733531993816));
#20353=CARTESIAN_POINT('',(8.3698219874924,1.7,8.47733531993816));
#20354=CARTESIAN_POINT('',(8.52266468006184,1.8,8.6301780125076));
#20355=CARTESIAN_POINT('Origin',(8.5857864376269,1.8,8.4142135623731));
#20356=CARTESIAN_POINT('',(8.52266468006184,2.1,8.6301780125076));
#20357=CARTESIAN_POINT('',(8.52266468006184,1.7,8.6301780125076));
#20358=CARTESIAN_POINT('Origin',(8.5857864376269,2.1,8.4142135623731));
#20359=CARTESIAN_POINT('Origin',(11.4142135623731,1.7,8.4142135623731));
#20360=CARTESIAN_POINT('',(11.4773353199382,1.8,8.6301780125076));
#20361=CARTESIAN_POINT('',(11.4773353199382,2.1,8.6301780125076));
#20362=CARTESIAN_POINT('',(11.4773353199382,1.7,8.6301780125076));
#20363=CARTESIAN_POINT('',(11.6301780125076,1.8,8.47733531993816));
#20364=CARTESIAN_POINT('Origin',(11.4142135623731,1.8,8.4142135623731));
#20365=CARTESIAN_POINT('',(11.6301780125076,2.1,8.47733531993816));
#20366=CARTESIAN_POINT('',(11.6301780125076,1.7,8.47733531993816));
#20367=CARTESIAN_POINT('Origin',(11.4142135623731,2.1,8.4142135623731));
#20368=CARTESIAN_POINT('Origin',(11.4142135623731,1.7,5.58578643762691));
#20369=CARTESIAN_POINT('',(11.6301780125076,1.8,5.52266468006184));
#20370=CARTESIAN_POINT('',(11.6301780125076,2.1,5.52266468006184));
#20371=CARTESIAN_POINT('',(11.6301780125076,1.7,5.52266468006184));
#20372=CARTESIAN_POINT('',(11.4773353199382,1.8,5.3698219874924));
#20373=CARTESIAN_POINT('Origin',(11.4142135623731,1.8,5.58578643762691));
#20374=CARTESIAN_POINT('',(11.4773353199382,2.1,5.3698219874924));
#20375=CARTESIAN_POINT('',(11.4773353199382,1.7,5.3698219874924));
#20376=CARTESIAN_POINT('Origin',(11.4142135623731,2.1,5.58578643762691));
#20377=CARTESIAN_POINT('Origin',(10.,1.8,7.));
#20378=CARTESIAN_POINT('Origin',(10.,1.8,7.));
#20379=CARTESIAN_POINT('Origin',(10.,1.8,7.));
#20380=CARTESIAN_POINT('Origin',(10.,1.8,7.));
#20381=CARTESIAN_POINT('Origin',(10.,1.8,7.));
#20382=CARTESIAN_POINT('',(8.41,1.8,7.));
#20383=CARTESIAN_POINT('Origin',(10.,1.8,7.));
#20384=CARTESIAN_POINT('Origin',(10.,1.8,7.));
#20385=CARTESIAN_POINT('Origin',(10.,2.1,7.));
#20386=CARTESIAN_POINT('Origin',(10.,1.8,7.));
#20387=CARTESIAN_POINT('Origin',(10.,2.1,7.));
#20388=CARTESIAN_POINT('Origin',(10.,1.8,7.));
#20389=CARTESIAN_POINT('Origin',(10.,2.1,7.));
#20390=CARTESIAN_POINT('Origin',(10.,1.8,7.));
#20391=CARTESIAN_POINT('Origin',(10.,2.1,7.));
#20392=CARTESIAN_POINT('Origin',(10.,1.4,7.));
#20393=CARTESIAN_POINT('',(8.41,1.4,7.));
#20394=CARTESIAN_POINT('',(8.41,1.4,7.));
#20395=CARTESIAN_POINT('Origin',(10.,1.4,7.));
#20396=CARTESIAN_POINT('Origin',(10.,1.4,7.));
#20397=CARTESIAN_POINT('',(8.8,1.4,7.));
#20398=CARTESIAN_POINT('Origin',(10.,1.4,7.));
#20399=CARTESIAN_POINT('Origin',(10.,1.8,7.));
#20400=CARTESIAN_POINT('',(8.8,2.1,7.));
#20401=CARTESIAN_POINT('Origin',(10.,2.1,7.));
#20402=CARTESIAN_POINT('',(8.8,1.8,7.));
#20403=CARTESIAN_POINT('Origin',(10.,2.1,7.));
#20404=CARTESIAN_POINT('',(0.,0.,0.));
#20405=CARTESIAN_POINT('Origin',(12.5,11.7,3.1));
#20406=CARTESIAN_POINT('',(12.335,11.7,3.2));
#20407=CARTESIAN_POINT('Origin',(12.5,11.7,3.2));
#20408=CARTESIAN_POINT('',(12.335,11.7,4.1));
#20409=CARTESIAN_POINT('',(12.335,11.7,3.1));
#20410=CARTESIAN_POINT('Origin',(12.5,11.7,4.1));
#20411=CARTESIAN_POINT('Origin',(12.5,11.7,4.1));
#20412=CARTESIAN_POINT('Origin',(11.5,10.3,3.1));
#20413=CARTESIAN_POINT('',(11.335,10.3,3.2));
#20414=CARTESIAN_POINT('Origin',(11.5,10.3,3.2));
#20415=CARTESIAN_POINT('',(11.335,10.3,4.1));
#20416=CARTESIAN_POINT('',(11.335,10.3,3.1));
#20417=CARTESIAN_POINT('Origin',(11.5,10.3,4.1));
#20418=CARTESIAN_POINT('Origin',(11.5,10.3,4.1));
#20419=CARTESIAN_POINT('Origin',(10.9,11.,4.5));
#20420=CARTESIAN_POINT('',(11.,11.,4.84));
#20421=CARTESIAN_POINT('Origin',(11.,11.,4.5));
#20422=CARTESIAN_POINT('',(13.,11.,4.84));
#20423=CARTESIAN_POINT('',(10.9,11.,4.84));
#20424=CARTESIAN_POINT('Origin',(13.,11.,4.5));
#20425=CARTESIAN_POINT('Origin',(13.,12.,3.2));
#20426=CARTESIAN_POINT('',(13.,12.,3.2));
#20427=CARTESIAN_POINT('',(11.,12.,3.2));
#20428=CARTESIAN_POINT('',(13.,12.,3.2));
#20429=CARTESIAN_POINT('',(11.,12.,5.7));
#20430=CARTESIAN_POINT('',(11.,12.,3.2));
#20431=CARTESIAN_POINT('',(13.,12.,5.7));
#20432=CARTESIAN_POINT('',(13.,12.,5.7));
#20433=CARTESIAN_POINT('',(13.,12.,3.2));
#20434=CARTESIAN_POINT('Origin',(13.,10.,3.2));
#20435=CARTESIAN_POINT('',(13.,10.,3.2));
#20436=CARTESIAN_POINT('',(13.,10.,3.2));
#20437=CARTESIAN_POINT('',(13.,10.,5.7));
#20438=CARTESIAN_POINT('',(13.,10.,5.7));
#20439=CARTESIAN_POINT('',(13.,10.,3.2));
#20440=CARTESIAN_POINT('Origin',(11.,10.,3.2));
#20441=CARTESIAN_POINT('',(11.,10.,3.2));
#20442=CARTESIAN_POINT('',(11.,10.,3.2));
#20443=CARTESIAN_POINT('',(11.,10.,5.7));
#20444=CARTESIAN_POINT('',(11.,10.,5.7));
#20445=CARTESIAN_POINT('',(11.,10.,3.2));
#20446=CARTESIAN_POINT('Origin',(11.,12.,3.2));
#20447=CARTESIAN_POINT('',(11.,12.,3.2));
#20448=CARTESIAN_POINT('',(11.,12.,5.7));
#20449=CARTESIAN_POINT('Origin',(12.,11.,5.7));
#20450=CARTESIAN_POINT('Origin',(12.,11.,3.2));
#20451=CARTESIAN_POINT('',(0.,0.,0.));
#20452=CARTESIAN_POINT('Origin',(14.,7.5,4.5));
#20453=CARTESIAN_POINT('',(14.,7.5,4.8));
#20454=CARTESIAN_POINT('Origin',(14.,7.5,4.5));
#20455=CARTESIAN_POINT('Origin',(3.,7.5,4.5));
#20456=CARTESIAN_POINT('',(3.,7.5,4.8));
#20457=CARTESIAN_POINT('',(3.,7.5,4.8));
#20458=CARTESIAN_POINT('Origin',(3.,7.5,4.5));
#20459=CARTESIAN_POINT('Origin',(3.,7.5,4.5));
#20460=CARTESIAN_POINT('',(0.,0.,0.));
#20461=CARTESIAN_POINT('Origin',(13.5,7.5,4.79));
#20462=CARTESIAN_POINT('',(13.3539691813349,7.42318854252131,4.79));
#20463=CARTESIAN_POINT('',(13.6460308186651,7.42318854252131,4.79));
#20464=CARTESIAN_POINT('',(12.9,7.42318854252131,4.79));
#20465=CARTESIAN_POINT('Origin',(13.5,7.5,4.79));
#20466=CARTESIAN_POINT('Origin',(13.5,7.5,4.79));
#20467=CARTESIAN_POINT('',(13.3539691813349,7.57681145747869,4.79));
#20468=CARTESIAN_POINT('',(13.335,7.5,4.8));
#20469=CARTESIAN_POINT('Ctrl Pts',(13.3539691813349,7.57681145747868,4.79));
#20470=CARTESIAN_POINT('Ctrl Pts',(13.3517424038809,7.57257799875687,4.79112130391241));
#20471=CARTESIAN_POINT('Ctrl Pts',(13.3496896532208,7.56822754447862,4.79217403693718));
#20472=CARTESIAN_POINT('Ctrl Pts',(13.3393317115009,7.54351674734392,4.79755094970157));
#20473=CARTESIAN_POINT('Ctrl Pts',(13.335,7.52120257394031,4.8));
#20474=CARTESIAN_POINT('Ctrl Pts',(13.335,7.5,4.8));
#20475=CARTESIAN_POINT('',(13.6460308186651,7.57681145747869,4.79));
#20476=CARTESIAN_POINT('Origin',(13.5,7.5,4.79));
#20477=CARTESIAN_POINT('',(13.665,7.5,4.8));
#20478=CARTESIAN_POINT('Ctrl Pts',(13.665,7.5,4.8));
#20479=CARTESIAN_POINT('Ctrl Pts',(13.665,7.52120257394031,4.8));
#20480=CARTESIAN_POINT('Ctrl Pts',(13.6606682884991,7.54351674734392,4.79755094970157));
#20481=CARTESIAN_POINT('Ctrl Pts',(13.6503103467792,7.56822754447862,4.79217403693718));
#20482=CARTESIAN_POINT('Ctrl Pts',(13.6482575961191,7.57257799875688,4.79112130391241));
#20483=CARTESIAN_POINT('Ctrl Pts',(13.6460308186651,7.57681145747869,4.79));
#20484=CARTESIAN_POINT('Ctrl Pts',(13.6460308186651,7.42318854252131,4.79));
#20485=CARTESIAN_POINT('Ctrl Pts',(13.6482575961191,7.42742200124312,4.79112130391241));
#20486=CARTESIAN_POINT('Ctrl Pts',(13.6503103467792,7.43177245552138,4.79217403693718));
#20487=CARTESIAN_POINT('Ctrl Pts',(13.6606682884991,7.45648325265608,4.79755094970157));
#20488=CARTESIAN_POINT('Ctrl Pts',(13.665,7.47879742605969,4.8));
#20489=CARTESIAN_POINT('Ctrl Pts',(13.665,7.5,4.8));
#20490=CARTESIAN_POINT('Ctrl Pts',(13.335,7.5,4.8));
#20491=CARTESIAN_POINT('Ctrl Pts',(13.335,7.47879742605969,4.8));
#20492=CARTESIAN_POINT('Ctrl Pts',(13.3393317115009,7.45648325265608,4.79755094970157));
#20493=CARTESIAN_POINT('Ctrl Pts',(13.3496896532208,7.43177245552138,4.79217403693718));
#20494=CARTESIAN_POINT('Ctrl Pts',(13.3517424038809,7.42742200124312,4.79112130391241));
#20495=CARTESIAN_POINT('Ctrl Pts',(13.3539691813349,7.42318854252132,4.79));
#20496=CARTESIAN_POINT('',(13.335,7.5,5.5));
#20497=CARTESIAN_POINT('',(13.335,7.5,4.79));
#20498=CARTESIAN_POINT('Origin',(13.5,7.5,5.5));
#20499=CARTESIAN_POINT('Origin',(13.5,7.5,4.79));
#20500=CARTESIAN_POINT('',(12.9,7.57681145747869,4.79));
#20501=CARTESIAN_POINT('Origin',(12.9,7.5,4.5));
#20502=CARTESIAN_POINT('',(13.,7.5,4.8));
#20503=CARTESIAN_POINT('Origin',(13.,7.5,4.5));
#20504=CARTESIAN_POINT('',(12.9,7.5,4.8));
#20505=CARTESIAN_POINT('',(14.,7.5,4.8));
#20506=CARTESIAN_POINT('',(12.9,7.5,4.8));
#20507=CARTESIAN_POINT('Origin',(14.,7.5,4.5));
#20508=CARTESIAN_POINT('Origin',(14.,8.5,3.2));
#20509=CARTESIAN_POINT('',(14.,8.5,3.2));
#20510=CARTESIAN_POINT('',(13.,8.5,3.2));
#20511=CARTESIAN_POINT('',(14.,8.5,3.2));
#20512=CARTESIAN_POINT('',(13.,8.5,5.5));
#20513=CARTESIAN_POINT('',(13.,8.5,3.2));
#20514=CARTESIAN_POINT('',(14.,8.5,5.5));
#20515=CARTESIAN_POINT('',(14.,8.5,5.5));
#20516=CARTESIAN_POINT('',(14.,8.5,3.2));
#20517=CARTESIAN_POINT('Origin',(14.,6.5,3.2));
#20518=CARTESIAN_POINT('',(14.,6.5,3.2));
#20519=CARTESIAN_POINT('',(14.,6.5,3.2));
#20520=CARTESIAN_POINT('',(14.,6.5,5.5));
#20521=CARTESIAN_POINT('',(14.,6.5,5.5));
#20522=CARTESIAN_POINT('',(14.,6.5,3.2));
#20523=CARTESIAN_POINT('Origin',(13.,6.5,3.2));
#20524=CARTESIAN_POINT('',(13.,6.5,3.2));
#20525=CARTESIAN_POINT('',(13.,6.5,3.2));
#20526=CARTESIAN_POINT('',(13.,6.5,5.5));
#20527=CARTESIAN_POINT('',(13.,6.5,5.5));
#20528=CARTESIAN_POINT('',(13.,6.5,3.2));
#20529=CARTESIAN_POINT('Origin',(13.,8.5,3.2));
#20530=CARTESIAN_POINT('',(13.,8.5,3.2));
#20531=CARTESIAN_POINT('',(13.,8.5,5.5));
#20532=CARTESIAN_POINT('Origin',(13.5,7.5,5.5));
#20533=CARTESIAN_POINT('Origin',(13.5,7.5,3.2));
#20534=CARTESIAN_POINT('',(0.,0.,0.));
#20535=CARTESIAN_POINT('',(0.,0.,0.));
#20536=CARTESIAN_POINT('Origin',(1.5,-1.9,1.7));
#20537=CARTESIAN_POINT('',(1.56403124237433,-1.7,1.7));
#20538=CARTESIAN_POINT('',(1.43596875762567,-1.7,1.7));
#20539=CARTESIAN_POINT('',(0.75,-1.7,1.7));
#20540=CARTESIAN_POINT('Origin',(1.5,-1.9,1.7));
#20541=CARTESIAN_POINT('Origin',(1.5,-1.9,1.7));
#20542=CARTESIAN_POINT('',(1.56403124237433,-1.7,1.75));
#20543=CARTESIAN_POINT('',(1.56403124237433,-1.7,1.7));
#20544=CARTESIAN_POINT('',(1.29,-1.9,1.75));
#20545=CARTESIAN_POINT('Origin',(1.5,-1.9,1.75));
#20546=CARTESIAN_POINT('',(1.29,-1.9,2.4));
#20547=CARTESIAN_POINT('',(1.29,-1.9,1.7));
#20548=CARTESIAN_POINT('Origin',(1.5,-1.9,2.4));
#20549=CARTESIAN_POINT('',(1.43596875762567,-1.7,1.75));
#20550=CARTESIAN_POINT('Origin',(1.5,-1.9,1.75));
#20551=CARTESIAN_POINT('',(1.43596875762567,-1.7,1.7));
#20552=CARTESIAN_POINT('Origin',(-1.5,1.9,1.7));
#20553=CARTESIAN_POINT('',(-1.56403124237433,1.7,1.7));
#20554=CARTESIAN_POINT('',(-1.43596875762567,1.7,1.7));
#20555=CARTESIAN_POINT('',(-0.75,1.7,1.7));
#20556=CARTESIAN_POINT('Origin',(-1.5,1.9,1.7));
#20557=CARTESIAN_POINT('Origin',(-1.5,1.9,1.7));
#20558=CARTESIAN_POINT('',(-1.56403124237433,1.7,1.75));
#20559=CARTESIAN_POINT('',(-1.56403124237433,1.7,1.7));
#20560=CARTESIAN_POINT('',(-1.71,1.9,1.75));
#20561=CARTESIAN_POINT('Origin',(-1.5,1.9,1.75));
#20562=CARTESIAN_POINT('',(-1.71,1.9,2.4));
#20563=CARTESIAN_POINT('',(-1.71,1.9,1.7));
#20564=CARTESIAN_POINT('Origin',(-1.5,1.9,2.4));
#20565=CARTESIAN_POINT('',(-1.43596875762567,1.7,1.75));
#20566=CARTESIAN_POINT('Origin',(-1.5,1.9,1.75));
#20567=CARTESIAN_POINT('',(-1.43596875762567,1.7,1.7));
#20568=CARTESIAN_POINT('Origin',(-1.5,-1.9,1.7));
#20569=CARTESIAN_POINT('',(-1.43596875762567,-1.7,1.7));
#20570=CARTESIAN_POINT('',(-1.56403124237433,-1.7,1.7));
#20571=CARTESIAN_POINT('',(-0.75,-1.7,1.7));
#20572=CARTESIAN_POINT('Origin',(-1.5,-1.9,1.7));
#20573=CARTESIAN_POINT('Origin',(-1.5,-1.9,1.7));
#20574=CARTESIAN_POINT('',(-1.43596875762567,-1.7,1.75));
#20575=CARTESIAN_POINT('',(-1.43596875762567,-1.7,1.7));
#20576=CARTESIAN_POINT('',(-1.71,-1.9,1.75));
#20577=CARTESIAN_POINT('Origin',(-1.5,-1.9,1.75));
#20578=CARTESIAN_POINT('',(-1.71,-1.9,2.4));
#20579=CARTESIAN_POINT('',(-1.71,-1.9,1.7));
#20580=CARTESIAN_POINT('Origin',(-1.5,-1.9,2.4));
#20581=CARTESIAN_POINT('',(-1.56403124237433,-1.7,1.75));
#20582=CARTESIAN_POINT('Origin',(-1.5,-1.9,1.75));
#20583=CARTESIAN_POINT('',(-1.56403124237433,-1.7,1.7));
#20584=CARTESIAN_POINT('Origin',(1.5,1.9,1.7));
#20585=CARTESIAN_POINT('',(1.43596875762567,1.7,1.7));
#20586=CARTESIAN_POINT('',(1.56403124237433,1.7,1.7));
#20587=CARTESIAN_POINT('',(0.75,1.7,1.7));
#20588=CARTESIAN_POINT('Origin',(1.5,1.9,1.7));
#20589=CARTESIAN_POINT('Origin',(1.5,1.9,1.7));
#20590=CARTESIAN_POINT('',(1.43596875762567,1.7,1.75));
#20591=CARTESIAN_POINT('',(1.43596875762567,1.7,1.7));
#20592=CARTESIAN_POINT('',(1.29,1.9,1.75));
#20593=CARTESIAN_POINT('Origin',(1.5,1.9,1.75));
#20594=CARTESIAN_POINT('',(1.29,1.9,2.4));
#20595=CARTESIAN_POINT('',(1.29,1.9,1.7));
#20596=CARTESIAN_POINT('Origin',(1.5,1.9,2.4));
#20597=CARTESIAN_POINT('',(1.56403124237433,1.7,1.75));
#20598=CARTESIAN_POINT('Origin',(1.5,1.9,1.75));
#20599=CARTESIAN_POINT('',(1.56403124237433,1.7,1.7));
#20600=CARTESIAN_POINT('Origin',(0.,-1.7,1.75));
#20601=CARTESIAN_POINT('',(0.,-1.7,1.75));
#20602=CARTESIAN_POINT('',(-1.97,-1.7,1.75));
#20603=CARTESIAN_POINT('',(0.,-1.7,1.75));
#20604=CARTESIAN_POINT('',(-1.97,-1.7,0.43));
#20605=CARTESIAN_POINT('',(-1.97,-1.7,1.75));
#20606=CARTESIAN_POINT('',(1.97,-1.7,0.43));
#20607=CARTESIAN_POINT('',(0.,-1.7,0.43));
#20608=CARTESIAN_POINT('',(1.97,-1.7,1.75));
#20609=CARTESIAN_POINT('',(1.97,-1.7,1.75));
#20610=CARTESIAN_POINT('',(0.,-1.7,1.75));
#20611=CARTESIAN_POINT('Origin',(0.,1.7,0.43));
#20612=CARTESIAN_POINT('',(0.,1.7,1.75));
#20613=CARTESIAN_POINT('',(1.97,1.7,1.75));
#20614=CARTESIAN_POINT('',(0.,1.7,1.75));
#20615=CARTESIAN_POINT('',(1.97,1.7,0.43));
#20616=CARTESIAN_POINT('',(1.97,1.7,0.43));
#20617=CARTESIAN_POINT('',(-1.97,1.7,0.43));
#20618=CARTESIAN_POINT('',(0.,1.7,0.43));
#20619=CARTESIAN_POINT('',(-1.97,1.7,1.75));
#20620=CARTESIAN_POINT('',(-1.97,1.7,0.43));
#20621=CARTESIAN_POINT('',(0.,1.7,1.75));
#20622=CARTESIAN_POINT('Origin',(-1.97,0.,1.415));
#20623=CARTESIAN_POINT('',(-1.97,-2.35,1.75));
#20624=CARTESIAN_POINT('',(-1.97,-2.35,1.75));
#20625=CARTESIAN_POINT('',(-1.97,-2.35,2.4));
#20626=CARTESIAN_POINT('',(-1.97,-2.35,2.4));
#20627=CARTESIAN_POINT('',(-1.97,2.35,2.4));
#20628=CARTESIAN_POINT('',(-1.97,2.35,2.4));
#20629=CARTESIAN_POINT('',(-1.97,2.35,1.75));
#20630=CARTESIAN_POINT('',(-1.97,2.35,1.75));
#20631=CARTESIAN_POINT('',(-1.97,1.7,1.75));
#20632=CARTESIAN_POINT('',(-1.97,0.78,0.43));
#20633=CARTESIAN_POINT('',(-1.97,0.78,0.43));
#20634=CARTESIAN_POINT('',(-1.97,0.78,1.55));
#20635=CARTESIAN_POINT('',(-1.97,0.78,1.55));
#20636=CARTESIAN_POINT('',(-1.97,-0.78,1.55));
#20637=CARTESIAN_POINT('',(-1.97,-0.78,1.55));
#20638=CARTESIAN_POINT('',(-1.97,-0.78,0.43));
#20639=CARTESIAN_POINT('',(-1.97,-0.78,0.43));
#20640=CARTESIAN_POINT('',(-1.97,-1.7,0.43));
#20641=CARTESIAN_POINT('Origin',(0.,-2.35,1.75));
#20642=CARTESIAN_POINT('',(1.97,-2.35,1.75));
#20643=CARTESIAN_POINT('',(1.97,-2.35,1.75));
#20644=CARTESIAN_POINT('',(0.,-2.35,1.75));
#20645=CARTESIAN_POINT('Origin',(0.,-2.35,2.4));
#20646=CARTESIAN_POINT('',(1.97,-2.35,2.4));
#20647=CARTESIAN_POINT('',(1.97,-2.35,2.4));
#20648=CARTESIAN_POINT('',(0.,-2.35,2.4));
#20649=CARTESIAN_POINT('Origin',(0.,2.35,2.4));
#20650=CARTESIAN_POINT('',(1.97,2.35,2.4));
#20651=CARTESIAN_POINT('',(1.97,2.35,2.4));
#20652=CARTESIAN_POINT('',(0.,2.35,2.4));
#20653=CARTESIAN_POINT('Origin',(0.,2.35,1.75));
#20654=CARTESIAN_POINT('',(1.97,2.35,1.75));
#20655=CARTESIAN_POINT('',(1.97,2.35,1.75));
#20656=CARTESIAN_POINT('',(0.,2.35,1.75));
#20657=CARTESIAN_POINT('Origin',(0.,1.7,1.75));
#20658=CARTESIAN_POINT('',(1.97,1.7,1.75));
#20659=CARTESIAN_POINT('Origin',(0.,0.78,0.43));
#20660=CARTESIAN_POINT('',(1.97,0.78,0.43));
#20661=CARTESIAN_POINT('',(1.97,0.78,0.43));
#20662=CARTESIAN_POINT('',(0.,0.78,0.43));
#20663=CARTESIAN_POINT('Origin',(0.,0.78,1.55));
#20664=CARTESIAN_POINT('',(1.97,0.78,1.55));
#20665=CARTESIAN_POINT('',(1.97,0.78,1.55));
#20666=CARTESIAN_POINT('',(0.,0.78,1.55));
#20667=CARTESIAN_POINT('Origin',(0.,-0.78,1.55));
#20668=CARTESIAN_POINT('',(1.97,-0.78,1.55));
#20669=CARTESIAN_POINT('',(1.97,-0.78,1.55));
#20670=CARTESIAN_POINT('',(0.,-0.78,1.55));
#20671=CARTESIAN_POINT('Origin',(0.,-0.78,0.43));
#20672=CARTESIAN_POINT('',(1.97,-0.78,0.43));
#20673=CARTESIAN_POINT('',(1.97,-0.78,0.43));
#20674=CARTESIAN_POINT('',(0.,-0.78,0.43));
#20675=CARTESIAN_POINT('Origin',(0.,-1.7,0.43));
#20676=CARTESIAN_POINT('',(1.97,-1.7,0.43));
#20677=CARTESIAN_POINT('Origin',(1.97,0.,1.415));
#20678=CARTESIAN_POINT('',(0.,0.,0.));
#20679=CARTESIAN_POINT('Origin',(1.97,1.7,2.3));
#20680=CARTESIAN_POINT('',(1.97,1.7,2.3));
#20681=CARTESIAN_POINT('',(1.97,-1.7,2.3));
#20682=CARTESIAN_POINT('',(1.97,1.7,2.3));
#20683=CARTESIAN_POINT('',(3.07,-1.7,2.3));
#20684=CARTESIAN_POINT('',(1.97,-1.7,2.3));
#20685=CARTESIAN_POINT('',(3.07,1.7,2.3));
#20686=CARTESIAN_POINT('',(3.07,1.7,2.3));
#20687=CARTESIAN_POINT('',(1.97,1.7,2.3));
#20688=CARTESIAN_POINT('Origin',(1.97,1.7,0.46));
#20689=CARTESIAN_POINT('',(1.97,1.7,0.46));
#20690=CARTESIAN_POINT('',(1.97,1.7,0.46));
#20691=CARTESIAN_POINT('',(3.07,1.7,0.46));
#20692=CARTESIAN_POINT('',(3.07,1.7,0.46));
#20693=CARTESIAN_POINT('',(1.97,1.7,0.46));
#20694=CARTESIAN_POINT('Origin',(1.97,0.78,0.46));
#20695=CARTESIAN_POINT('',(1.97,0.78,0.46));
#20696=CARTESIAN_POINT('',(1.97,0.78,0.46));
#20697=CARTESIAN_POINT('',(3.07,0.78,0.46));
#20698=CARTESIAN_POINT('',(3.07,0.78,0.46));
#20699=CARTESIAN_POINT('',(1.97,0.78,0.46));
#20700=CARTESIAN_POINT('Origin',(1.97,0.78,1.55));
#20701=CARTESIAN_POINT('',(1.97,0.78,1.55));
#20702=CARTESIAN_POINT('',(1.97,0.78,1.55));
#20703=CARTESIAN_POINT('',(3.07,0.78,1.55));
#20704=CARTESIAN_POINT('',(3.07,0.78,1.55));
#20705=CARTESIAN_POINT('',(1.97,0.78,1.55));
#20706=CARTESIAN_POINT('Origin',(1.97,-0.78,1.55));
#20707=CARTESIAN_POINT('',(1.97,-0.78,1.55));
#20708=CARTESIAN_POINT('',(1.97,-0.78,1.55));
#20709=CARTESIAN_POINT('',(3.07,-0.78,1.55));
#20710=CARTESIAN_POINT('',(3.07,-0.78,1.55));
#20711=CARTESIAN_POINT('',(1.97,-0.78,1.55));
#20712=CARTESIAN_POINT('Origin',(1.97,-0.78,0.46));
#20713=CARTESIAN_POINT('',(1.97,-0.78,0.46));
#20714=CARTESIAN_POINT('',(1.97,-0.78,0.46));
#20715=CARTESIAN_POINT('',(3.07,-0.78,0.46));
#20716=CARTESIAN_POINT('',(3.07,-0.78,0.46));
#20717=CARTESIAN_POINT('',(1.97,-0.78,0.46));
#20718=CARTESIAN_POINT('Origin',(1.97,-1.7,0.46));
#20719=CARTESIAN_POINT('',(1.97,-1.7,0.46));
#20720=CARTESIAN_POINT('',(1.97,-1.7,0.46));
#20721=CARTESIAN_POINT('',(3.07,-1.7,0.46));
#20722=CARTESIAN_POINT('',(3.07,-1.7,0.46));
#20723=CARTESIAN_POINT('',(1.97,-1.7,0.46));
#20724=CARTESIAN_POINT('Origin',(1.97,-1.7,2.3));
#20725=CARTESIAN_POINT('',(1.97,-1.7,2.3));
#20726=CARTESIAN_POINT('',(3.07,-1.7,2.3));
#20727=CARTESIAN_POINT('Origin',(3.07,0.,1.38));
#20728=CARTESIAN_POINT('Origin',(1.97,0.,1.38));
#20729=CARTESIAN_POINT('',(0.,0.,0.));
#20730=CARTESIAN_POINT('Origin',(-1.97,-0.78,0.46));
#20731=CARTESIAN_POINT('',(-1.97,-1.7,0.46));
#20732=CARTESIAN_POINT('',(-1.97,-0.78,0.46));
#20733=CARTESIAN_POINT('',(-1.97,-1.7,0.46));
#20734=CARTESIAN_POINT('',(-3.07,-1.7,0.46));
#20735=CARTESIAN_POINT('',(-1.97,-1.7,0.46));
#20736=CARTESIAN_POINT('',(-3.07,-0.78,0.46));
#20737=CARTESIAN_POINT('',(-3.07,-1.7,0.46));
#20738=CARTESIAN_POINT('',(-1.97,-0.78,0.46));
#20739=CARTESIAN_POINT('Origin',(-1.97,-0.78,1.55));
#20740=CARTESIAN_POINT('',(-1.97,-0.78,1.55));
#20741=CARTESIAN_POINT('',(-1.97,-0.78,0.46));
#20742=CARTESIAN_POINT('',(-3.07,-0.78,1.55));
#20743=CARTESIAN_POINT('',(-3.07,-0.78,0.46));
#20744=CARTESIAN_POINT('',(-1.97,-0.78,1.55));
#20745=CARTESIAN_POINT('Origin',(-1.97,0.78,1.55));
#20746=CARTESIAN_POINT('',(-1.97,0.78,1.55));
#20747=CARTESIAN_POINT('',(-1.97,-0.78,1.55));
#20748=CARTESIAN_POINT('',(-3.07,0.78,1.55));
#20749=CARTESIAN_POINT('',(-3.07,-0.78,1.55));
#20750=CARTESIAN_POINT('',(-1.97,0.78,1.55));
#20751=CARTESIAN_POINT('Origin',(-1.97,0.78,0.46));
#20752=CARTESIAN_POINT('',(-1.97,0.78,0.46));
#20753=CARTESIAN_POINT('',(-1.97,0.78,1.55));
#20754=CARTESIAN_POINT('',(-3.07,0.78,0.46));
#20755=CARTESIAN_POINT('',(-3.07,0.78,1.55));
#20756=CARTESIAN_POINT('',(-1.97,0.78,0.46));
#20757=CARTESIAN_POINT('Origin',(-1.97,1.7,0.46));
#20758=CARTESIAN_POINT('',(-1.97,1.7,0.46));
#20759=CARTESIAN_POINT('',(-1.97,0.78,0.46));
#20760=CARTESIAN_POINT('',(-3.07,1.7,0.46));
#20761=CARTESIAN_POINT('',(-3.07,0.78,0.46));
#20762=CARTESIAN_POINT('',(-1.97,1.7,0.46));
#20763=CARTESIAN_POINT('Origin',(-1.97,1.7,2.3));
#20764=CARTESIAN_POINT('',(-1.97,1.7,2.3));
#20765=CARTESIAN_POINT('',(-1.97,1.7,0.46));
#20766=CARTESIAN_POINT('',(-3.07,1.7,2.3));
#20767=CARTESIAN_POINT('',(-3.07,1.7,0.46));
#20768=CARTESIAN_POINT('',(-1.97,1.7,2.3));
#20769=CARTESIAN_POINT('Origin',(-1.97,-1.7,2.3));
#20770=CARTESIAN_POINT('',(-1.97,-1.7,2.3));
#20771=CARTESIAN_POINT('',(-1.97,1.7,2.3));
#20772=CARTESIAN_POINT('',(-3.07,-1.7,2.3));
#20773=CARTESIAN_POINT('',(-3.07,1.7,2.3));
#20774=CARTESIAN_POINT('',(-1.97,-1.7,2.3));
#20775=CARTESIAN_POINT('Origin',(-1.97,-1.7,0.46));
#20776=CARTESIAN_POINT('',(-1.97,-1.7,2.3));
#20777=CARTESIAN_POINT('',(-3.07,-1.7,2.3));
#20778=CARTESIAN_POINT('Origin',(-1.97,0.,1.38));
#20779=CARTESIAN_POINT('Origin',(-3.07,0.,1.38));
#20780=CARTESIAN_POINT('',(0.,0.,0.));
#20781=CARTESIAN_POINT('',(0.,0.,0.));
#20782=CARTESIAN_POINT('',(0.,0.,0.));
#20783=CARTESIAN_POINT('',(0.,0.,0.));
#20784=CARTESIAN_POINT('Origin',(0.115470053837925,-0.5,-0.2));
#20785=CARTESIAN_POINT('',(0.23094010767585,-0.5,0.));
#20786=CARTESIAN_POINT('',(0.115470053837925,-0.5,-0.2));
#20787=CARTESIAN_POINT('',(0.23094010767585,-0.5,0.));
#20788=CARTESIAN_POINT('',(0.115470053837925,-0.8,-0.2));
#20789=CARTESIAN_POINT('',(0.115470053837925,-0.5,-0.2));
#20790=CARTESIAN_POINT('',(0.23094010767585,-0.8,0.));
#20791=CARTESIAN_POINT('',(0.23094010767585,-0.8,0.));
#20792=CARTESIAN_POINT('',(0.23094010767585,-0.5,0.));
#20793=CARTESIAN_POINT('Origin',(-0.115470053837925,-0.5,-0.2));
#20794=CARTESIAN_POINT('',(-0.115470053837925,-0.5,-0.2));
#20795=CARTESIAN_POINT('',(0.115470053837925,-0.5,-0.2));
#20796=CARTESIAN_POINT('',(-0.115470053837925,-0.8,-0.2));
#20797=CARTESIAN_POINT('',(-0.115470053837925,-0.5,-0.2));
#20798=CARTESIAN_POINT('',(0.115470053837925,-0.8,-0.2));
#20799=CARTESIAN_POINT('Origin',(-0.23094010767585,-0.5,-2.77555756156289E-17));
#20800=CARTESIAN_POINT('',(-0.23094010767585,-0.5,-2.82820063659975E-17));
#20801=CARTESIAN_POINT('',(-0.115470053837925,-0.5,-0.2));
#20802=CARTESIAN_POINT('',(-0.23094010767585,-0.8,-2.77555756156289E-17));
#20803=CARTESIAN_POINT('',(-0.23094010767585,-0.5,-2.82820063659975E-17));
#20804=CARTESIAN_POINT('',(-0.115470053837925,-0.8,-0.2));
#20805=CARTESIAN_POINT('Origin',(-0.115470053837925,-0.5,0.2));
#20806=CARTESIAN_POINT('',(-0.115470053837925,-0.5,0.2));
#20807=CARTESIAN_POINT('',(-0.23094010767585,-0.5,-2.82820063659975E-17));
#20808=CARTESIAN_POINT('',(-0.115470053837925,-0.8,0.2));
#20809=CARTESIAN_POINT('',(-0.115470053837925,-0.5,0.2));
#20810=CARTESIAN_POINT('',(-0.23094010767585,-0.8,-2.82820063659975E-17));
#20811=CARTESIAN_POINT('Origin',(0.115470053837925,-0.5,0.2));
#20812=CARTESIAN_POINT('',(0.115470053837925,-0.5,0.2));
#20813=CARTESIAN_POINT('',(-0.115470053837925,-0.5,0.2));
#20814=CARTESIAN_POINT('',(0.115470053837925,-0.8,0.2));
#20815=CARTESIAN_POINT('',(0.115470053837925,-0.5,0.2));
#20816=CARTESIAN_POINT('',(-0.115470053837925,-0.8,0.2));
#20817=CARTESIAN_POINT('Origin',(0.23094010767585,-0.5,0.));
#20818=CARTESIAN_POINT('',(0.115470053837925,-0.5,0.2));
#20819=CARTESIAN_POINT('',(0.115470053837925,-0.8,0.2));
#20820=CARTESIAN_POINT('Origin',(0.,-0.5,0.));
#20821=CARTESIAN_POINT('Origin',(0.,-0.8,0.));
#20822=CARTESIAN_POINT('Origin',(0.,-1.4,0.));
#20823=CARTESIAN_POINT('',(-0.24505,-1.4,3.00099698131059E-17));
#20824=CARTESIAN_POINT('Origin',(0.,-1.4,0.));
#20825=CARTESIAN_POINT('Origin',(0.375,0.5,0.));
#20826=CARTESIAN_POINT('',(-0.375,0.5,-4.59242549680257E-17));
#20827=CARTESIAN_POINT('Origin',(0.,0.5,0.));
#20828=CARTESIAN_POINT('Origin',(0.,0.475,0.));
#20829=CARTESIAN_POINT('',(-0.425,0.45,-5.20474889637625E-17));
#20830=CARTESIAN_POINT('Origin',(0.,0.45,0.));
#20831=CARTESIAN_POINT('',(-0.4,0.475,-4.89858719658941E-17));
#20832=CARTESIAN_POINT('Origin',(0.,0.24,0.));
#20833=CARTESIAN_POINT('',(-0.425,0.0299999999999998,-5.20474889637625E-17));
#20834=CARTESIAN_POINT('Origin',(0.,0.0299999999999998,0.));
#20835=CARTESIAN_POINT('',(-0.425,0.24,-5.20474889637625E-17));
#20836=CARTESIAN_POINT('Origin',(0.,0.0150000000000001,0.));
#20837=CARTESIAN_POINT('',(-0.395,4.85722573273506E-17,-4.83735485663204E-17));
#20838=CARTESIAN_POINT('Origin',(0.,0.,0.));
#20839=CARTESIAN_POINT('',(-0.41,0.0150000000000001,-5.02105187650415E-17));
#20840=CARTESIAN_POINT('Origin',(0.27,0.,0.));
#20841=CARTESIAN_POINT('',(-0.27,0.,-3.30654635769785E-17));
#20842=CARTESIAN_POINT('Origin',(0.,0.,0.));
#20843=CARTESIAN_POINT('Origin',(0.,-0.02,0.));
#20844=CARTESIAN_POINT('',(-0.24505,-0.0498999999999999,3.00099698131059E-17));
#20845=CARTESIAN_POINT('Origin',(0.,-0.0498999999999999,0.));
#20846=CARTESIAN_POINT('',(-0.26,-0.02,-3.18408167778312E-17));
#20847=CARTESIAN_POINT('Origin',(0.,-0.995,0.));
#20848=CARTESIAN_POINT('',(-0.24505,-0.995,-3.00099698131059E-17));
#20849=CARTESIAN_POINT('',(0.,0.,0.));
#20850=CARTESIAN_POINT('',(0.,0.,0.));
#20851=CARTESIAN_POINT('Origin',(0.,0.,0.));
#20852=CARTESIAN_POINT('',(-1.070235,-0.308121667383195,-1.31065986708547E-16));
#20853=CARTESIAN_POINT('',(-1.31065986708547E-16,-0.308121667383195,1.070235));
#20854=CARTESIAN_POINT('Origin',(0.,-0.308121667383195,0.));
#20855=CARTESIAN_POINT('Origin',(0.,-0.308121667383195,0.));
#20856=CARTESIAN_POINT('',(-1.31065986708547E-16,0.308121667383195,1.070235));
#20857=CARTESIAN_POINT('Origin',(-1.34711147906209E-16,0.,1.1));
#20858=CARTESIAN_POINT('',(-1.070235,0.308121667383195,1.31065986708547E-16));
#20859=CARTESIAN_POINT('Origin',(0.,0.308121667383195,0.));
#20860=CARTESIAN_POINT('Origin',(0.,0.308121667383195,0.));
#20861=CARTESIAN_POINT('Origin',(0.,0.,0.));
#20862=CARTESIAN_POINT('',(-1.070235,0.5,-1.31065986708547E-16));
#20863=CARTESIAN_POINT('',(-1.070235,0.,-1.31065986708547E-16));
#20864=CARTESIAN_POINT('Origin',(0.,0.5,0.));
#20865=CARTESIAN_POINT('Origin',(0.,0.,0.));
#20866=CARTESIAN_POINT('',(-0.6,-0.44,-7.34788079488412E-17));
#20867=CARTESIAN_POINT('Origin',(0.,-0.44,0.));
#20868=CARTESIAN_POINT('',(-0.6,0.44,-7.34788079488412E-17));
#20869=CARTESIAN_POINT('',(-0.6,0.,-7.34788079488412E-17));
#20870=CARTESIAN_POINT('Origin',(0.,0.44,0.));
#20871=CARTESIAN_POINT('Origin',(0.,0.47,0.));
#20872=CARTESIAN_POINT('',(-0.66,0.5,-8.08266887437253E-17));
#20873=CARTESIAN_POINT('',(-0.63,0.47,-7.71527483462832E-17));
#20874=CARTESIAN_POINT('Origin',(0.,0.5,0.));
#20875=CARTESIAN_POINT('Origin',(1.070235,0.5,0.));
#20876=CARTESIAN_POINT('Origin',(0.,0.,0.));
#20877=CARTESIAN_POINT('',(-1.070235,-0.5,-1.31065986708547E-16));
#20878=CARTESIAN_POINT('Origin',(0.,-0.5,0.));
#20879=CARTESIAN_POINT('',(-1.070235,0.,-1.31065986708547E-16));
#20880=CARTESIAN_POINT('Origin',(0.66,-0.5,0.));
#20881=CARTESIAN_POINT('',(-0.66,-0.5,-8.08266887437253E-17));
#20882=CARTESIAN_POINT('Origin',(0.,-0.5,0.));
#20883=CARTESIAN_POINT('Origin',(0.,-0.47,0.));
#20884=CARTESIAN_POINT('',(-0.63,-0.47,-7.71527483462832E-17));
#20885=CARTESIAN_POINT('',(0.,0.,0.));
#20886=CARTESIAN_POINT('Origin',(0.,0.,0.));
#20887=CARTESIAN_POINT('',(-1.129765,0.308121667383195,-1.38356309103871E-16));
#20888=CARTESIAN_POINT('',(-1.38356309103871E-16,0.308121667383195,1.129765));
#20889=CARTESIAN_POINT('Origin',(0.,0.308121667383195,0.));
#20890=CARTESIAN_POINT('Origin',(0.,0.308121667383195,0.));
#20891=CARTESIAN_POINT('',(-1.38356309103871E-16,-0.308121667383195,1.129765));
#20892=CARTESIAN_POINT('Origin',(-1.34711147906209E-16,0.,1.1));
#20893=CARTESIAN_POINT('',(-1.129765,-0.308121667383195,1.38356309103871E-16));
#20894=CARTESIAN_POINT('Origin',(0.,-0.308121667383195,0.));
#20895=CARTESIAN_POINT('Origin',(0.,-0.308121667383195,0.));
#20896=CARTESIAN_POINT('Origin',(0.,0.,0.));
#20897=CARTESIAN_POINT('',(-1.129765,-0.5,-1.38356309103871E-16));
#20898=CARTESIAN_POINT('Origin',(0.,-0.5,0.));
#20899=CARTESIAN_POINT('',(-1.129765,0.,-1.38356309103871E-16));
#20900=CARTESIAN_POINT('Origin',(1.54,0.5,0.));
#20901=CARTESIAN_POINT('',(-1.54,0.5,-1.88595607068692E-16));
#20902=CARTESIAN_POINT('Origin',(0.,0.5,0.));
#20903=CARTESIAN_POINT('',(-1.129765,0.5,-1.38356309103871E-16));
#20904=CARTESIAN_POINT('Origin',(0.,0.5,0.));
#20905=CARTESIAN_POINT('Origin',(0.,0.47,0.));
#20906=CARTESIAN_POINT('',(-1.6,0.44,-1.95943487863577E-16));
#20907=CARTESIAN_POINT('Origin',(0.,0.44,0.));
#20908=CARTESIAN_POINT('',(-1.57,0.47,-1.92269547466134E-16));
#20909=CARTESIAN_POINT('Origin',(0.,0.,0.));
#20910=CARTESIAN_POINT('',(-1.6,-0.44,-1.95943487863577E-16));
#20911=CARTESIAN_POINT('Origin',(0.,-0.44,0.));
#20912=CARTESIAN_POINT('',(-1.6,0.,-1.95943487863577E-16));
#20913=CARTESIAN_POINT('Origin',(0.,-0.47,0.));
#20914=CARTESIAN_POINT('',(-1.54,-0.5,-1.88595607068692E-16));
#20915=CARTESIAN_POINT('Origin',(0.,-0.5,0.));
#20916=CARTESIAN_POINT('',(-1.57,-0.47,-1.92269547466134E-16));
#20917=CARTESIAN_POINT('Origin',(1.129765,-0.5,0.));
#20918=CARTESIAN_POINT('Origin',(0.,0.,0.));
#20919=CARTESIAN_POINT('',(-1.129765,0.,-1.38356309103871E-16));
#20920=CARTESIAN_POINT('',(0.,0.,0.));
#20921=CARTESIAN_POINT('Origin',(1.1,0.,0.));
#20922=CARTESIAN_POINT('',(1.1,-2.23201749654651E-33,0.29765));
#20923=CARTESIAN_POINT('',(1.1,-2.23201749654651E-33,-0.29765));
#20924=CARTESIAN_POINT('Origin',(1.1,0.,0.));
#20925=CARTESIAN_POINT('Origin',(0.685838782044607,0.,-0.860014630714833));
#20926=CARTESIAN_POINT('',(0.918550922801216,-5.31350540756609E-33,-0.674432891191581));
#20927=CARTESIAN_POINT('',(0.453126641287998,8.49470414473068E-34,-1.04559637023808));
#20928=CARTESIAN_POINT('Origin',(0.685838782044607,0.,-0.860014630714833));
#20929=CARTESIAN_POINT('Origin',(-0.244773027351946,0.,-1.07242070340001));
#20930=CARTESIAN_POINT('',(0.0454142657089739,-2.23201749654651E-33,-1.1386540593921));
#20931=CARTESIAN_POINT('',(-0.534960320412865,-2.23201749654651E-33,-1.00618734740791));
#20932=CARTESIAN_POINT('Origin',(-0.244773027351946,0.,-1.07242070340001));
#20933=CARTESIAN_POINT('Origin',(-0.991065754692661,0.,-0.477272113029314));
#20934=CARTESIAN_POINT('',(-0.86192025974432,8.49470414473067E-34,-0.745445496560469));
#20935=CARTESIAN_POINT('',(-1.120211249641,-5.31350540756609E-33,-0.209098729498159));
#20936=CARTESIAN_POINT('Origin',(-0.991065754692661,0.,-0.477272113029314));
#20937=CARTESIAN_POINT('Origin',(-0.991065754692661,0.,0.477272113029314));
#20938=CARTESIAN_POINT('',(-1.120211249641,-2.23201749654651E-33,0.209098729498159));
#20939=CARTESIAN_POINT('',(-0.86192025974432,-2.23201749654651E-33,0.745445496560469));
#20940=CARTESIAN_POINT('Origin',(-0.991065754692661,0.,0.477272113029314));
#20941=CARTESIAN_POINT('Origin',(-0.244773027351946,0.,1.07242070340001));
#20942=CARTESIAN_POINT('',(-0.534960320412866,-2.23201749654651E-33,1.00618734740791));
#20943=CARTESIAN_POINT('',(0.0454142657089737,-2.23201749654651E-33,1.1386540593921));
#20944=CARTESIAN_POINT('Origin',(-0.244773027351946,0.,1.07242070340001));
#20945=CARTESIAN_POINT('Origin',(0.685838782044607,0.,0.860014630714833));
#20946=CARTESIAN_POINT('',(0.453126641287998,-2.23201749654651E-33,1.04559637023808));
#20947=CARTESIAN_POINT('',(0.918550922801216,-2.23201749654651E-33,0.674432891191581));
#20948=CARTESIAN_POINT('Origin',(0.685838782044607,0.,0.860014630714833));
#20949=CARTESIAN_POINT('',(0.,0.,0.));
#20950=CARTESIAN_POINT('Origin',(0.685838782044607,0.,0.860014630714833));
#20951=CARTESIAN_POINT('',(0.413083465285518,-0.05953,0.993751811093549));
#20952=CARTESIAN_POINT('',(0.876916659919095,-0.05953,0.623857181492959));
#20953=CARTESIAN_POINT('Ctrl Pts',(0.413083465285518,-0.05953,0.993751811093549));
#20954=CARTESIAN_POINT('Ctrl Pts',(0.419070565453383,-0.0925528133349865,
0.991263089003441));
#20955=CARTESIAN_POINT('Ctrl Pts',(0.430199341854858,-0.124911173756694,
0.986608710139579));
#20956=CARTESIAN_POINT('Ctrl Pts',(0.457978755888596,-0.177924977804098,
0.973971221090534));
#20957=CARTESIAN_POINT('Ctrl Pts',(0.473077587363685,-0.199697230012983,
0.966820759530997));
#20958=CARTESIAN_POINT('Ctrl Pts',(0.507057380724533,-0.237895043532788,
0.949440676105255));
#20959=CARTESIAN_POINT('Ctrl Pts',(0.525933334162555,-0.254319232363049,
0.939198248544428));
#20960=CARTESIAN_POINT('Ctrl Pts',(0.564362943424238,-0.28018331644634,
0.916597376014514));
#20961=CARTESIAN_POINT('Ctrl Pts',(0.585840553788742,-0.29104845371857,
0.903141581680914));
#20962=CARTESIAN_POINT('Ctrl Pts',(0.629305439856167,-0.30527573347708,
0.873412008702649));
#20963=CARTESIAN_POINT('Ctrl Pts',(0.651278921914856,-0.308638795020976,
0.857118508332695));
#20964=CARTESIAN_POINT('Ctrl Pts',(0.690705563850638,-0.308638795020976,
0.825676810575914));
#20965=CARTESIAN_POINT('Ctrl Pts',(0.711480111898423,-0.30527573347708,
0.807879894508811));
#20966=CARTESIAN_POINT('Ctrl Pts',(0.750136149454208,-0.29104845371857,
0.772120216227122));
#20967=CARTESIAN_POINT('Ctrl Pts',(0.768033796848072,-0.28018331644634,
0.754175290318038));
#20968=CARTESIAN_POINT('Ctrl Pts',(0.798619410861634,-0.254319232363049,
0.721738358858166));
#20969=CARTESIAN_POINT('Ctrl Pts',(0.812805334167529,-0.237895043532788,
0.705614819529209));
#20970=CARTESIAN_POINT('Ctrl Pts',(0.837310877969633,-0.199697230012983,
0.676354402927683));
#20971=CARTESIAN_POINT('Ctrl Pts',(0.847641868610495,-0.177924977804098,
0.663225258065736));
#20972=CARTESIAN_POINT('Ctrl Pts',(0.866144010579847,-0.124911173756694,
0.638954437806245));
#20973=CARTESIAN_POINT('Ctrl Pts',(0.873158080166742,-0.0925528133349865,
0.62914037979579));
#20974=CARTESIAN_POINT('Ctrl Pts',(0.876916659919095,-0.05953,0.623857181492959));
#20975=CARTESIAN_POINT('',(0.437601487681057,-0.05953,1.03511272300331));
#20976=CARTESIAN_POINT('Origin',(0.685838782044607,-0.05953,0.860014630714833));
#20977=CARTESIAN_POINT('',(0.911784794170997,-0.05953,0.656964154625313));
#20978=CARTESIAN_POINT('Ctrl Pts',(0.911784794170998,-0.0595300000000001,
0.656964154625312));
#20979=CARTESIAN_POINT('Ctrl Pts',(0.909827729890942,-0.0762225747374255,
0.659680317203144));
#20980=CARTESIAN_POINT('Ctrl Pts',(0.907004864562642,-0.0928409665394228,
0.663576540841106));
#20981=CARTESIAN_POINT('Ctrl Pts',(0.895234408667242,-0.144299303100741,
0.679480524217551));
#20982=CARTESIAN_POINT('Ctrl Pts',(0.882797231409153,-0.177024326825049,
0.695831250979106));
#20983=CARTESIAN_POINT('Ctrl Pts',(0.854332839576145,-0.227269801620064,
0.73042219438957));
#20984=CARTESIAN_POINT('Ctrl Pts',(0.834863020612702,-0.251265615809407,
0.752807465209441));
#20985=CARTESIAN_POINT('Ctrl Pts',(0.800439809856111,-0.279889827963178,
0.789147407129766));
#20986=CARTESIAN_POINT('Ctrl Pts',(0.781998747691871,-0.290879136862659,
0.80756613568454));
#20987=CARTESIAN_POINT('Ctrl Pts',(0.742239891936898,-0.305251990234487,
0.844254137480382));
#20988=CARTESIAN_POINT('Ctrl Pts',(0.720906778729541,-0.308638795020976,
0.862505527716294));
#20989=CARTESIAN_POINT('Ctrl Pts',(0.680463863683392,-0.308638795020976,
0.894757676234429));
#20990=CARTESIAN_POINT('Ctrl Pts',(0.657923009631182,-0.305251990234488,
0.91149460735272));
#20991=CARTESIAN_POINT('Ctrl Pts',(0.613307674922609,-0.290879136862659,
0.942092777160053));
#20992=CARTESIAN_POINT('Ctrl Pts',(0.591247219971725,-0.279889827963178,
0.955972930713954));
#20993=CARTESIAN_POINT('Ctrl Pts',(0.548158511259202,-0.251265615809407,
0.981446681891443));
#20994=CARTESIAN_POINT('Ctrl Pts',(0.522002043615455,-0.227269801620063,
0.995447160474328));
#20995=CARTESIAN_POINT('Ctrl Pts',(0.481944444320713,-0.177024326825049,
1.01550068154148));
#20996=CARTESIAN_POINT('Ctrl Pts',(0.463236132117164,-0.14429930310074,
1.0239876538093));
#20997=CARTESIAN_POINT('Ctrl Pts',(0.445111721969657,-0.0928409665394226,
1.03192403056628));
#20998=CARTESIAN_POINT('Ctrl Pts',(0.440685038163619,-0.0762225747374254,
1.03380912944435));
#20999=CARTESIAN_POINT('Ctrl Pts',(0.437601487681056,-0.05953,1.03511272300331));
#21000=CARTESIAN_POINT('Origin',(0.685838782044607,-0.05953,0.860014630714833));
#21001=CARTESIAN_POINT('Origin',(0.,-0.208355,0.));
#21002=CARTESIAN_POINT('',(0.0548532617164168,-0.05953,1.12247250791415));
#21003=CARTESIAN_POINT('Origin',(0.,-0.05953,0.));
#21004=CARTESIAN_POINT('',(-0.536443649899848,-0.05953,0.987512846410683));
#21005=CARTESIAN_POINT('Ctrl Pts',(0.0548532617164173,-0.0595300000000001,
1.12247250791414));
#21006=CARTESIAN_POINT('Ctrl Pts',(0.05150947068137,-0.0762225747374254,
1.12263591311425));
#21007=CARTESIAN_POINT('Ctrl Pts',(0.0467032526342597,-0.0928409665394227,
1.12285816383385));
#21008=CARTESIAN_POINT('Ctrl Pts',(0.0269302585198975,-0.144299303100741,
1.12357162229597));
#21009=CARTESIAN_POINT('Ctrl Pts',(0.006392292392153,-0.177024326825049,
1.12404235695137));
#21010=CARTESIAN_POINT('Ctrl Pts',(-0.0383992541984087,-0.227269801620063,
1.12335509974011));
#21011=CARTESIAN_POINT('Ctrl Pts',(-0.0680399972366993,-0.251265615809407,
1.12208997038458));
#21012=CARTESIAN_POINT('Ctrl Pts',(-0.117914228755037,-0.279889827963178,
1.1178344036749));
#21013=CARTESIAN_POINT('Ctrl Pts',(-0.14381238480104,-0.290879136862659,
1.11490049012186));
#21014=CARTESIAN_POINT('Ctrl Pts',(-0.19728546073067,-0.305251990234488,
1.10669035995599));
#21015=CARTESIAN_POINT('Ctrl Pts',(-0.224855950742601,-0.308638795020976,
1.10139101611326));
#21016=CARTESIAN_POINT('Ctrl Pts',(-0.275287440920027,-0.308638795020976,
1.0898803575765));
#21017=CARTESIAN_POINT('Ctrl Pts',(-0.302426893214945,-0.305251990234488,
1.08269251410343));
#21018=CARTESIAN_POINT('Ctrl Pts',(-0.35416671187353,-0.290879136862659,
1.06688848765783));
#21019=CARTESIAN_POINT('Ctrl Pts',(-0.3787731215897,-0.279889827963178,
1.05829506364875));
#21020=CARTESIAN_POINT('Ctrl Pts',(-0.425554672694338,-0.251265615809407,
1.04048957871266));
#21021=CARTESIAN_POINT('Ctrl Pts',(-0.452808978448581,-0.227269801620063,
1.02876878445619));
#21022=CARTESIAN_POINT('Ctrl Pts',(-0.493462957200432,-0.177024326825049,
1.0099536580922));
#21023=CARTESIAN_POINT('Ctrl Pts',(-0.511762781179148,-0.14429930310074,
1.00061845128527));
#21024=CARTESIAN_POINT('Ctrl Pts',(-0.529268075276157,-0.0928409665394226,
0.991396466802468));
#21025=CARTESIAN_POINT('Ctrl Pts',(-0.533501897135713,-0.0762225747374254,
0.989110885965947));
#21026=CARTESIAN_POINT('Ctrl Pts',(-0.536443649899848,-0.0595300000000001,
0.987512846410683));
#21027=CARTESIAN_POINT('',(-0.843383895613249,-0.05953,0.742736168477219));
#21028=CARTESIAN_POINT('Origin',(0.,-0.05953,0.));
#21029=CARTESIAN_POINT('',(-1.10653577764992,-0.05953,0.196295654879792));
#21030=CARTESIAN_POINT('Ctrl Pts',(-0.843383895613249,-0.0595300000000001,
0.742736168477219));
#21031=CARTESIAN_POINT('Ctrl Pts',(-0.84559647055299,-0.0762225747374255,
0.740223768851062));
#21032=CARTESIAN_POINT('Ctrl Pts',(-0.848766861100456,-0.0928409665394227,
0.736604687327351));
#21033=CARTESIAN_POINT('Ctrl Pts',(-0.861652925570091,-0.144299303100741,
0.721590372101268));
#21034=CARTESIAN_POINT('Ctrl Pts',(-0.87482617317514,-0.177024326825049,
0.705826641853758));
#21035=CARTESIAN_POINT('Ctrl Pts',(-0.902215926359523,-0.227269801620063,
0.670378702718353));
#21036=CARTESIAN_POINT('Ctrl Pts',(-0.919707509403859,-0.251265615809407,
0.646415841396062));
#21037=CARTESIAN_POINT('Ctrl Pts',(-0.947476448101718,-0.279889827963178,
0.604769294586516));
#21038=CARTESIAN_POINT('Ctrl Pts',(-0.961329858300736,-0.290879136862659,
0.582692035672022));
#21039=CARTESIAN_POINT('Ctrl Pts',(-0.988250837578047,-0.305251990234488,
0.535766169015486));
#21040=CARTESIAN_POINT('Ctrl Pts',(-1.00129756308006,-0.308638795020976,
0.510906605094603));
#21041=CARTESIAN_POINT('Ctrl Pts',(-1.02374168767024,-0.308638795020976,
0.46430090015576));
#21042=CARTESIAN_POINT('Ctrl Pts',(-1.03504317708586,-0.305251990234488,
0.438600874831839));
#21043=CARTESIAN_POINT('Ctrl Pts',(-1.05494634094458,-0.290879136862659,
0.388295406390235));
#21044=CARTESIAN_POINT('Ctrl Pts',(-1.06356957703048,-0.279889827963178,
0.363699428370917));
#21045=CARTESIAN_POINT('Ctrl Pts',(-1.0788165083757,-0.251265615809407,
0.316022600643821));
#21046=CARTESIAN_POINT('Ctrl Pts',(-1.08664560412098,-0.227269801620063,
0.287406530683752));
#21047=CARTESIAN_POINT('Ctrl Pts',(-1.09728268713976,-0.177024326825049,
0.243890930799337));
#21048=CARTESIAN_POINT('Ctrl Pts',(-1.10139388218929,-0.144299303100741,
0.22376314604679));
#21049=CARTESIAN_POINT('Ctrl Pts',(-1.10509821673782,-0.0928409665394227,
0.204327142733961));
#21050=CARTESIAN_POINT('Ctrl Pts',(-1.10595102243643,-0.0762225747374254,
0.199591971170104));
#21051=CARTESIAN_POINT('Ctrl Pts',(-1.10653577764992,-0.0595300000000001,
0.196295654879792));
#21052=CARTESIAN_POINT('',(-1.123812,-0.05953,1.37627276864339E-16));
#21053=CARTESIAN_POINT('Origin',(0.,-0.05953,0.));
#21054=CARTESIAN_POINT('',(-1.123812,-0.35718,1.37627276864339E-16));
#21055=CARTESIAN_POINT('',(-1.123812,-0.208355,1.37627276864339E-16));
#21056=CARTESIAN_POINT('Origin',(0.,-0.35718,0.));
#21057=CARTESIAN_POINT('',(-1.10653577764992,-0.05953,-0.196295654879793));
#21058=CARTESIAN_POINT('Origin',(0.,-0.05953,0.));
#21059=CARTESIAN_POINT('',(-0.843383895613249,-0.05953,-0.742736168477219));
#21060=CARTESIAN_POINT('Ctrl Pts',(-1.10653577764992,-0.0595300000000001,
-0.196295654879792));
#21061=CARTESIAN_POINT('Ctrl Pts',(-1.10595102243643,-0.0762225747374255,
-0.199591971170104));
#21062=CARTESIAN_POINT('Ctrl Pts',(-1.10509821673782,-0.0928409665394228,
-0.204327142733962));
#21063=CARTESIAN_POINT('Ctrl Pts',(-1.10139388218929,-0.144299303100741,
-0.22376314604679));
#21064=CARTESIAN_POINT('Ctrl Pts',(-1.09728268713976,-0.177024326825049,
-0.243890930799338));
#21065=CARTESIAN_POINT('Ctrl Pts',(-1.08664560412098,-0.227269801620063,
-0.287406530683753));
#21066=CARTESIAN_POINT('Ctrl Pts',(-1.0788165083757,-0.251265615809407,
-0.316022600643821));
#21067=CARTESIAN_POINT('Ctrl Pts',(-1.06356957703048,-0.279889827963178,
-0.363699428370918));
#21068=CARTESIAN_POINT('Ctrl Pts',(-1.05494634094458,-0.290879136862659,
-0.388295406390235));
#21069=CARTESIAN_POINT('Ctrl Pts',(-1.03504317708586,-0.305251990234488,
-0.438600874831839));
#21070=CARTESIAN_POINT('Ctrl Pts',(-1.02374168767024,-0.308638795020976,
-0.46430090015576));
#21071=CARTESIAN_POINT('Ctrl Pts',(-1.00129756308006,-0.308638795020976,
-0.510906605094603));
#21072=CARTESIAN_POINT('Ctrl Pts',(-0.988250837578047,-0.305251990234488,
-0.535766169015486));
#21073=CARTESIAN_POINT('Ctrl Pts',(-0.961329858300736,-0.290879136862659,
-0.582692035672022));
#21074=CARTESIAN_POINT('Ctrl Pts',(-0.947476448101718,-0.279889827963178,
-0.604769294586516));
#21075=CARTESIAN_POINT('Ctrl Pts',(-0.919707509403859,-0.251265615809407,
-0.646415841396062));
#21076=CARTESIAN_POINT('Ctrl Pts',(-0.902215926359523,-0.227269801620064,
-0.670378702718353));
#21077=CARTESIAN_POINT('Ctrl Pts',(-0.87482617317514,-0.177024326825049,
-0.705826641853758));
#21078=CARTESIAN_POINT('Ctrl Pts',(-0.861652925570091,-0.144299303100741,
-0.721590372101268));
#21079=CARTESIAN_POINT('Ctrl Pts',(-0.848766861100456,-0.0928409665394229,
-0.736604687327351));
#21080=CARTESIAN_POINT('Ctrl Pts',(-0.84559647055299,-0.0762225747374255,
-0.740223768851063));
#21081=CARTESIAN_POINT('Ctrl Pts',(-0.843383895613249,-0.0595300000000001,
-0.742736168477219));
#21082=CARTESIAN_POINT('',(-0.536443649899847,-0.05953,-0.987512846410683));
#21083=CARTESIAN_POINT('Origin',(0.,-0.05953,0.));
#21084=CARTESIAN_POINT('',(0.0548532617164172,-0.05953,-1.12247250791415));
#21085=CARTESIAN_POINT('Ctrl Pts',(-0.536443649899848,-0.0595300000000001,
-0.987512846410683));
#21086=CARTESIAN_POINT('Ctrl Pts',(-0.533501897135712,-0.0762225747374254,
-0.989110885965947));
#21087=CARTESIAN_POINT('Ctrl Pts',(-0.529268075276156,-0.0928409665394227,
-0.991396466802469));
#21088=CARTESIAN_POINT('Ctrl Pts',(-0.511762781179147,-0.144299303100741,
-1.00061845128527));
#21089=CARTESIAN_POINT('Ctrl Pts',(-0.493462957200432,-0.177024326825049,
-1.0099536580922));
#21090=CARTESIAN_POINT('Ctrl Pts',(-0.45280897844858,-0.227269801620063,
-1.02876878445619));
#21091=CARTESIAN_POINT('Ctrl Pts',(-0.425554672694337,-0.251265615809407,
-1.04048957871266));
#21092=CARTESIAN_POINT('Ctrl Pts',(-0.3787731215897,-0.279889827963178,
-1.05829506364875));
#21093=CARTESIAN_POINT('Ctrl Pts',(-0.354166711873529,-0.290879136862659,
-1.06688848765783));
#21094=CARTESIAN_POINT('Ctrl Pts',(-0.302426893214944,-0.305251990234488,
-1.08269251410343));
#21095=CARTESIAN_POINT('Ctrl Pts',(-0.275287440920027,-0.308638795020976,
-1.0898803575765));
#21096=CARTESIAN_POINT('Ctrl Pts',(-0.224855950742601,-0.308638795020976,
-1.10139101611326));
#21097=CARTESIAN_POINT('Ctrl Pts',(-0.19728546073067,-0.305251990234488,
-1.10669035995599));
#21098=CARTESIAN_POINT('Ctrl Pts',(-0.143812384801039,-0.290879136862659,
-1.11490049012186));
#21099=CARTESIAN_POINT('Ctrl Pts',(-0.117914228755037,-0.279889827963178,
-1.1178344036749));
#21100=CARTESIAN_POINT('Ctrl Pts',(-0.0680399972366989,-0.251265615809407,
-1.12208997038458));
#21101=CARTESIAN_POINT('Ctrl Pts',(-0.0383992541984084,-0.227269801620063,
-1.12335509974011));
#21102=CARTESIAN_POINT('Ctrl Pts',(0.00639229239215326,-0.177024326825049,
-1.12404235695137));
#21103=CARTESIAN_POINT('Ctrl Pts',(0.0269302585198977,-0.144299303100741,
-1.12357162229597));
#21104=CARTESIAN_POINT('Ctrl Pts',(0.04670325263426,-0.0928409665394228,
-1.12285816383385));
#21105=CARTESIAN_POINT('Ctrl Pts',(0.0515094706813703,-0.0762225747374255,
-1.12263591311425));
#21106=CARTESIAN_POINT('Ctrl Pts',(0.0548532617164176,-0.0595300000000001,
-1.12247250791414));
#21107=CARTESIAN_POINT('',(0.437601487681057,-0.05953,-1.03511272300331));
#21108=CARTESIAN_POINT('Origin',(0.,-0.05953,0.));
#21109=CARTESIAN_POINT('',(0.911784794170997,-0.05953,-0.656964154625313));
#21110=CARTESIAN_POINT('Ctrl Pts',(0.437601487681056,-0.0595300000000001,
-1.03511272300331));
#21111=CARTESIAN_POINT('Ctrl Pts',(0.440685038163619,-0.0762225747374255,
-1.03380912944435));
#21112=CARTESIAN_POINT('Ctrl Pts',(0.445111721969657,-0.0928409665394228,
-1.03192403056628));
#21113=CARTESIAN_POINT('Ctrl Pts',(0.463236132117164,-0.144299303100741,
-1.0239876538093));
#21114=CARTESIAN_POINT('Ctrl Pts',(0.481944444320713,-0.177024326825049,
-1.01550068154148));
#21115=CARTESIAN_POINT('Ctrl Pts',(0.522002043615455,-0.227269801620064,
-0.995447160474328));
#21116=CARTESIAN_POINT('Ctrl Pts',(0.548158511259203,-0.251265615809407,
-0.981446681891443));
#21117=CARTESIAN_POINT('Ctrl Pts',(0.591247219971725,-0.279889827963178,
-0.955972930713954));
#21118=CARTESIAN_POINT('Ctrl Pts',(0.613307674922609,-0.290879136862659,
-0.942092777160053));
#21119=CARTESIAN_POINT('Ctrl Pts',(0.657923009631182,-0.305251990234487,
-0.91149460735272));
#21120=CARTESIAN_POINT('Ctrl Pts',(0.680463863683393,-0.308638795020976,
-0.894757676234429));
#21121=CARTESIAN_POINT('Ctrl Pts',(0.720906778729542,-0.308638795020976,
-0.862505527716294));
#21122=CARTESIAN_POINT('Ctrl Pts',(0.742239891936899,-0.305251990234488,
-0.844254137480381));
#21123=CARTESIAN_POINT('Ctrl Pts',(0.781998747691872,-0.290879136862659,
-0.80756613568454));
#21124=CARTESIAN_POINT('Ctrl Pts',(0.800439809856112,-0.279889827963178,
-0.789147407129765));
#21125=CARTESIAN_POINT('Ctrl Pts',(0.834863020612702,-0.251265615809407,
-0.752807465209441));
#21126=CARTESIAN_POINT('Ctrl Pts',(0.854332839576145,-0.227269801620064,
-0.73042219438957));
#21127=CARTESIAN_POINT('Ctrl Pts',(0.882797231409153,-0.177024326825049,
-0.695831250979106));
#21128=CARTESIAN_POINT('Ctrl Pts',(0.895234408667242,-0.144299303100741,
-0.679480524217551));
#21129=CARTESIAN_POINT('Ctrl Pts',(0.907004864562642,-0.0928409665394228,
-0.663576540841106));
#21130=CARTESIAN_POINT('Ctrl Pts',(0.909827729890942,-0.0762225747374256,
-0.659680317203144));
#21131=CARTESIAN_POINT('Ctrl Pts',(0.911784794170998,-0.0595300000000001,
-0.656964154625312));
#21132=CARTESIAN_POINT('',(1.08212377959455,-0.05953,-0.303251606722892));
#21133=CARTESIAN_POINT('Origin',(0.,-0.05953,0.));
#21134=CARTESIAN_POINT('',(1.08212377959455,-0.05953,0.303251606722892));
#21135=CARTESIAN_POINT('Ctrl Pts',(1.08212377959455,-0.0595300000000001,
-0.303251606722892));
#21136=CARTESIAN_POINT('Ctrl Pts',(1.0830271513892,-0.0762225747374255,
-0.300028012588062));
#21137=CARTESIAN_POINT('Ctrl Pts',(1.08431331394788,-0.0928409665394228,
-0.2953917518996));
#21138=CARTESIAN_POINT('Ctrl Pts',(1.08940878963422,-0.144299303100741,
-0.276273267473431));
#21139=CARTESIAN_POINT('Ctrl Pts',(1.09443784939331,-0.177024326825049,
-0.256354979351213));
#21140=CARTESIAN_POINT('Ctrl Pts',(1.10373487993589,-0.227269801620064,
-0.212533521233765));
#21141=CARTESIAN_POINT('Ctrl Pts',(1.10909715583869,-0.251265615809407,
-0.183354415742157));
#21142=CARTESIAN_POINT('Ctrl Pts',(1.1160463456491,-0.279889827963178,-0.133783682657561));
#21143=CARTESIAN_POINT('Ctrl Pts',(1.11894887330541,-0.290879136862659,
-0.107881990270302));
#21144=CARTESIAN_POINT('Ctrl Pts',(1.12284346704144,-0.305251990234488,
-0.0539226701638766));
#21145=CARTESIAN_POINT('Ctrl Pts',(1.123812,-0.308638795020976,-0.025864214957475));
#21146=CARTESIAN_POINT('Ctrl Pts',(1.123812,-0.308638795020976,0.025864214957475));
#21147=CARTESIAN_POINT('Ctrl Pts',(1.12284346704144,-0.305251990234488,
0.0539226701638766));
#21148=CARTESIAN_POINT('Ctrl Pts',(1.11894887330541,-0.290879136862659,
0.107881990270302));
#21149=CARTESIAN_POINT('Ctrl Pts',(1.1160463456491,-0.279889827963178,0.133783682657561));
#21150=CARTESIAN_POINT('Ctrl Pts',(1.10909715583869,-0.251265615809407,
0.183354415742157));
#21151=CARTESIAN_POINT('Ctrl Pts',(1.10373487993589,-0.227269801620064,
0.212533521233765));
#21152=CARTESIAN_POINT('Ctrl Pts',(1.09443784939331,-0.177024326825049,
0.256354979351213));
#21153=CARTESIAN_POINT('Ctrl Pts',(1.08940878963422,-0.144299303100741,
0.276273267473431));
#21154=CARTESIAN_POINT('Ctrl Pts',(1.08431331394788,-0.0928409665394228,
0.2953917518996));
#21155=CARTESIAN_POINT('Ctrl Pts',(1.0830271513892,-0.0762225747374255,
0.300028012588062));
#21156=CARTESIAN_POINT('Ctrl Pts',(1.08212377959455,-0.0595300000000001,
0.303251606722892));
#21157=CARTESIAN_POINT('Origin',(0.,-0.05953,0.));
#21158=CARTESIAN_POINT('Origin',(0.,-0.05953,0.));
#21159=CARTESIAN_POINT('',(0.0589974094846122,-0.05953,1.07456964270265));
#21160=CARTESIAN_POINT('Origin',(0.,-0.05953,0.));
#21161=CARTESIAN_POINT('Origin',(-0.244773027351946,-0.05953,1.07242070340001));
#21162=CARTESIAN_POINT('Origin',(-0.244773027351946,0.,1.07242070340001));
#21163=CARTESIAN_POINT('',(-0.519393123750572,-0.05953,0.942555777842682));
#21164=CARTESIAN_POINT('Ctrl Pts',(-0.519393123750572,-0.05953,0.942555777842682));
#21165=CARTESIAN_POINT('Ctrl Pts',(-0.513714466572041,-0.0925528133349865,
0.945684988399766));
#21166=CARTESIAN_POINT('Ctrl Pts',(-0.503136848051455,-0.124911173756694,
0.951483858396181));
#21167=CARTESIAN_POINT('Ctrl Pts',(-0.47593627990192,-0.177924977804098,
0.965323333309091));
#21168=CARTESIAN_POINT('Ctrl Pts',(-0.460931856495794,-0.199697230012983,
0.972669835243841));
#21169=CARTESIAN_POINT('Ctrl Pts',(-0.426157505475872,-0.237895043532788,
0.988400002689705));
#21170=CARTESIAN_POINT('Ctrl Pts',(-0.406380688682952,-0.254319232363049,
0.996771768218699));
#21171=CARTESIAN_POINT('Ctrl Pts',(-0.364750145543744,-0.28018331644634,
1.01272583306292));
#21172=CARTESIAN_POINT('Ctrl Pts',(-0.340838910881557,-0.29104845371857,
1.02112815447116));
#21173=CARTESIAN_POINT('Ctrl Pts',(-0.290495481564827,-0.30527573347708,
1.036574285215));
#21174=CARTESIAN_POINT('Ctrl Pts',(-0.264056468041074,-0.308638795020976,
1.04359501395068));
#21175=CARTESIAN_POINT('Ctrl Pts',(-0.214892249704082,-0.308638795020976,
1.05481642595959));
#21176=CARTESIAN_POINT('Ctrl Pts',(-0.188025341585962,-0.30527573347708,
1.05996242598502));
#21177=CARTESIAN_POINT('Ctrl Pts',(-0.135965654106109,-0.29104845371857,
1.06788913840721));
#21178=CARTESIAN_POINT('Ctrl Pts',(-0.110776745452494,-0.28018331644634,
1.07069360430242));
#21179=CARTESIAN_POINT('Ctrl Pts',(-0.0663467128214646,-0.254319232363049,
1.07438230428002));
#21180=CARTESIAN_POINT('Ctrl Pts',(-0.0448960436540983,-0.237895043532788,
1.07542044338697));
#21181=CARTESIAN_POINT('Ctrl Pts',(-0.00674037211528124,-0.199697230012983,
1.07633607767727));
#21182=CARTESIAN_POINT('Ctrl Pts',(0.00996567398334777,-0.177924977804098,
1.07622728347683));
#21183=CARTESIAN_POINT('Ctrl Pts',(0.0404772621979741,-0.124911173756694,
1.07556023164702));
#21184=CARTESIAN_POINT('Ctrl Pts',(0.0525234025782719,-0.0925528133349865,
1.07492508698591));
#21185=CARTESIAN_POINT('Ctrl Pts',(0.0589974094846124,-0.05953,1.07456964270265));
#21186=CARTESIAN_POINT('Origin',(-0.244773027351946,-0.05953,1.07242070340001));
#21187=CARTESIAN_POINT('Origin',(0.,-0.05953,0.));
#21188=CARTESIAN_POINT('',(-0.803348093619616,-0.05953,0.716109245731214));
#21189=CARTESIAN_POINT('Origin',(0.,-0.05953,0.));
#21190=CARTESIAN_POINT('Origin',(-0.991065754692661,-0.05953,0.477272113029314));
#21191=CARTESIAN_POINT('Origin',(-0.991065754692661,0.,0.477272113029314));
#21192=CARTESIAN_POINT('',(-1.06075609691358,-0.05953,0.181596019242328));
#21193=CARTESIAN_POINT('Ctrl Pts',(-1.06075609691358,-0.05953,0.181596019242328));
#21194=CARTESIAN_POINT('Ctrl Pts',(-1.05966202740332,-0.0925528133349865,
0.187986803072856));
#21195=CARTESIAN_POINT('Ctrl Pts',(-1.05760072925372,-0.124911173756694,
0.199872254546857));
#21196=CARTESIAN_POINT('Ctrl Pts',(-1.05146158959546,-0.177924977804098,
0.22976728653846));
#21197=CARTESIAN_POINT('Ctrl Pts',(-1.04785021111757,-0.199697230012983,
0.246078686169301));
#21198=CARTESIAN_POINT('Ctrl Pts',(-1.03846709802406,-0.237895043532788,
0.283073967563097));
#21199=CARTESIAN_POINT('Ctrl Pts',(-1.03268176429485,-0.254319232363049,
0.303755815985685));
#21200=CARTESIAN_POINT('Ctrl Pts',(-1.01919893537026,-0.28018331644634,
0.346251081972725));
#21201=CARTESIAN_POINT('Ctrl Pts',(-1.01085972381132,-0.29104845371857,
0.370184399726282));
#21202=CARTESIAN_POINT('Ctrl Pts',(-0.99154738033959,-0.30527573347708,
0.419174982698463));
#21203=CARTESIAN_POINT('Ctrl Pts',(-0.980551951791748,-0.308638795020976,
0.444223188605045));
#21204=CARTESIAN_POINT('Ctrl Pts',(-0.958671816228589,-0.308638795020976,
0.489657758261848));
#21205=CARTESIAN_POINT('Ctrl Pts',(-0.945943877838127,-0.30527573347708,
0.51387163140139));
#21206=CARTESIAN_POINT('Ctrl Pts',(-0.91968254693063,-0.29104845371857,
0.559515758398093));
#21207=CARTESIAN_POINT('Ctrl Pts',(-0.906170138993533,-0.28018331644634,
0.580957796077825));
#21208=CARTESIAN_POINT('Ctrl Pts',(-0.8813524085237,-0.254319232363049,
0.617994461173994));
#21209=CARTESIAN_POINT('Ctrl Pts',(-0.868789784891799,-0.237895043532788,
0.635412538795143));
#21210=CARTESIAN_POINT('Ctrl Pts',(-0.845715984518854,-0.199697230012983,
0.66581473268113));
#21211=CARTESIAN_POINT('Ctrl Pts',(-0.835214876415962,-0.177924977804098,
0.678808213394124));
#21212=CARTESIAN_POINT('Ctrl Pts',(-0.815669690204649,-0.124911173756694,
0.702247233627224));
#21213=CARTESIAN_POINT('Ctrl Pts',(-0.807662468433796,-0.0925528133349865,
0.711269279199861));
#21214=CARTESIAN_POINT('Ctrl Pts',(-0.803348093619616,-0.05953,0.716109245731214));
#21215=CARTESIAN_POINT('Origin',(-0.991065754692661,-0.05953,0.477272113029314));
#21216=CARTESIAN_POINT('Origin',(0.,-0.05953,0.));
#21217=CARTESIAN_POINT('',(-1.076188,-0.05953,1.31795018948079E-16));
#21218=CARTESIAN_POINT('Origin',(0.,-0.05953,0.));
#21219=CARTESIAN_POINT('',(-1.06075609691358,-0.05953,-0.181596019242328));
#21220=CARTESIAN_POINT('Origin',(0.,-0.05953,0.));
#21221=CARTESIAN_POINT('Origin',(-0.991065754692661,-0.05953,-0.477272113029314));
#21222=CARTESIAN_POINT('Origin',(-0.991065754692661,0.,-0.477272113029314));
#21223=CARTESIAN_POINT('',(-0.803348093619616,-0.05953,-0.716109245731215));
#21224=CARTESIAN_POINT('Ctrl Pts',(-0.803348093619616,-0.05953,-0.716109245731215));
#21225=CARTESIAN_POINT('Ctrl Pts',(-0.807662468433795,-0.0925528133349865,
-0.711269279199862));
#21226=CARTESIAN_POINT('Ctrl Pts',(-0.815669690204649,-0.124911173756694,
-0.702247233627224));
#21227=CARTESIAN_POINT('Ctrl Pts',(-0.835214876415962,-0.177924977804098,
-0.678808213394124));
#21228=CARTESIAN_POINT('Ctrl Pts',(-0.845715984518854,-0.199697230012983,
-0.66581473268113));
#21229=CARTESIAN_POINT('Ctrl Pts',(-0.868789784891799,-0.237895043532788,
-0.635412538795143));
#21230=CARTESIAN_POINT('Ctrl Pts',(-0.8813524085237,-0.254319232363049,
-0.617994461173994));
#21231=CARTESIAN_POINT('Ctrl Pts',(-0.906170138993533,-0.28018331644634,
-0.580957796077826));
#21232=CARTESIAN_POINT('Ctrl Pts',(-0.91968254693063,-0.29104845371857,
-0.559515758398093));
#21233=CARTESIAN_POINT('Ctrl Pts',(-0.945943877838127,-0.30527573347708,
-0.51387163140139));
#21234=CARTESIAN_POINT('Ctrl Pts',(-0.958671816228589,-0.308638795020976,
-0.489657758261848));
#21235=CARTESIAN_POINT('Ctrl Pts',(-0.980551951791748,-0.308638795020976,
-0.444223188605045));
#21236=CARTESIAN_POINT('Ctrl Pts',(-0.99154738033959,-0.30527573347708,
-0.419174982698463));
#21237=CARTESIAN_POINT('Ctrl Pts',(-1.01085972381132,-0.29104845371857,
-0.370184399726282));
#21238=CARTESIAN_POINT('Ctrl Pts',(-1.01919893537026,-0.28018331644634,
-0.346251081972725));
#21239=CARTESIAN_POINT('Ctrl Pts',(-1.03268176429485,-0.254319232363049,
-0.303755815985685));
#21240=CARTESIAN_POINT('Ctrl Pts',(-1.03846709802406,-0.237895043532788,
-0.283073967563097));
#21241=CARTESIAN_POINT('Ctrl Pts',(-1.04785021111757,-0.199697230012983,
-0.246078686169302));
#21242=CARTESIAN_POINT('Ctrl Pts',(-1.05146158959546,-0.177924977804098,
-0.229767286538461));
#21243=CARTESIAN_POINT('Ctrl Pts',(-1.05760072925372,-0.124911173756694,
-0.199872254546858));
#21244=CARTESIAN_POINT('Ctrl Pts',(-1.05966202740332,-0.0925528133349864,
-0.187986803072857));
#21245=CARTESIAN_POINT('Ctrl Pts',(-1.06075609691358,-0.05953,-0.181596019242328));
#21246=CARTESIAN_POINT('Origin',(-0.991065754692661,-0.05953,-0.477272113029314));
#21247=CARTESIAN_POINT('Origin',(0.,-0.05953,0.));
#21248=CARTESIAN_POINT('',(-0.519393123750572,-0.05953,-0.942555777842682));
#21249=CARTESIAN_POINT('Origin',(0.,-0.05953,0.));
#21250=CARTESIAN_POINT('Origin',(-0.244773027351946,-0.05953,-1.07242070340001));
#21251=CARTESIAN_POINT('Origin',(-0.244773027351946,0.,-1.07242070340001));
#21252=CARTESIAN_POINT('',(0.0589974094846125,-0.05953,-1.07456964270265));
#21253=CARTESIAN_POINT('Ctrl Pts',(0.0589974094846127,-0.05953,-1.07456964270265));
#21254=CARTESIAN_POINT('Ctrl Pts',(0.0525234025782722,-0.0925528133349865,
-1.07492508698591));
#21255=CARTESIAN_POINT('Ctrl Pts',(0.0404772621979744,-0.124911173756694,
-1.07556023164702));
#21256=CARTESIAN_POINT('Ctrl Pts',(0.0099656739833481,-0.177924977804098,
-1.07622728347683));
#21257=CARTESIAN_POINT('Ctrl Pts',(-0.00674037211528096,-0.199697230012983,
-1.07633607767727));
#21258=CARTESIAN_POINT('Ctrl Pts',(-0.044896043654098,-0.237895043532788,
-1.07542044338697));
#21259=CARTESIAN_POINT('Ctrl Pts',(-0.0663467128214644,-0.254319232363049,
-1.07438230428002));
#21260=CARTESIAN_POINT('Ctrl Pts',(-0.110776745452493,-0.28018331644634,
-1.07069360430242));
#21261=CARTESIAN_POINT('Ctrl Pts',(-0.135965654106109,-0.29104845371857,
-1.06788913840721));
#21262=CARTESIAN_POINT('Ctrl Pts',(-0.188025341585962,-0.30527573347708,
-1.05996242598502));
#21263=CARTESIAN_POINT('Ctrl Pts',(-0.214892249704082,-0.308638795020976,
-1.05481642595959));
#21264=CARTESIAN_POINT('Ctrl Pts',(-0.264056468041074,-0.308638795020976,
-1.04359501395068));
#21265=CARTESIAN_POINT('Ctrl Pts',(-0.290495481564827,-0.30527573347708,
-1.036574285215));
#21266=CARTESIAN_POINT('Ctrl Pts',(-0.340838910881557,-0.291048453718569,
-1.02112815447116));
#21267=CARTESIAN_POINT('Ctrl Pts',(-0.364750145543744,-0.28018331644634,
-1.01272583306292));
#21268=CARTESIAN_POINT('Ctrl Pts',(-0.406380688682952,-0.254319232363049,
-0.996771768218699));
#21269=CARTESIAN_POINT('Ctrl Pts',(-0.426157505475872,-0.237895043532788,
-0.988400002689705));
#21270=CARTESIAN_POINT('Ctrl Pts',(-0.460931856495794,-0.199697230012983,
-0.972669835243841));
#21271=CARTESIAN_POINT('Ctrl Pts',(-0.475936279901919,-0.177924977804098,
-0.965323333309091));
#21272=CARTESIAN_POINT('Ctrl Pts',(-0.503136848051454,-0.124911173756694,
-0.951483858396181));
#21273=CARTESIAN_POINT('Ctrl Pts',(-0.513714466572041,-0.0925528133349865,
-0.945684988399766));
#21274=CARTESIAN_POINT('Ctrl Pts',(-0.519393123750572,-0.05953,-0.942555777842682));
#21275=CARTESIAN_POINT('Origin',(-0.244773027351946,-0.05953,-1.07242070340001));
#21276=CARTESIAN_POINT('Origin',(0.,-0.05953,0.));
#21277=CARTESIAN_POINT('',(0.413083465285518,-0.05953,-0.993751811093549));
#21278=CARTESIAN_POINT('Origin',(0.,-0.05953,0.));
#21279=CARTESIAN_POINT('Origin',(0.685838782044607,-0.05953,-0.860014630714833));
#21280=CARTESIAN_POINT('Origin',(0.685838782044607,0.,-0.860014630714833));
#21281=CARTESIAN_POINT('',(0.876916659919095,-0.05953,-0.623857181492959));
#21282=CARTESIAN_POINT('Ctrl Pts',(0.876916659919095,-0.05953,-0.623857181492958));
#21283=CARTESIAN_POINT('Ctrl Pts',(0.873158080166742,-0.0925528133349865,
-0.62914037979579));
#21284=CARTESIAN_POINT('Ctrl Pts',(0.866144010579847,-0.124911173756694,
-0.638954437806245));
#21285=CARTESIAN_POINT('Ctrl Pts',(0.847641868610495,-0.177924977804098,
-0.663225258065736));
#21286=CARTESIAN_POINT('Ctrl Pts',(0.837310877969633,-0.199697230012983,
-0.676354402927683));
#21287=CARTESIAN_POINT('Ctrl Pts',(0.81280533416753,-0.237895043532788,
-0.705614819529209));
#21288=CARTESIAN_POINT('Ctrl Pts',(0.798619410861634,-0.254319232363049,
-0.721738358858166));
#21289=CARTESIAN_POINT('Ctrl Pts',(0.768033796848072,-0.28018331644634,
-0.754175290318038));
#21290=CARTESIAN_POINT('Ctrl Pts',(0.750136149454208,-0.29104845371857,
-0.772120216227122));
#21291=CARTESIAN_POINT('Ctrl Pts',(0.711480111898423,-0.30527573347708,
-0.807879894508811));
#21292=CARTESIAN_POINT('Ctrl Pts',(0.690705563850638,-0.308638795020976,
-0.825676810575913));
#21293=CARTESIAN_POINT('Ctrl Pts',(0.651278921914856,-0.308638795020976,
-0.857118508332695));
#21294=CARTESIAN_POINT('Ctrl Pts',(0.629305439856167,-0.30527573347708,
-0.873412008702649));
#21295=CARTESIAN_POINT('Ctrl Pts',(0.585840553788742,-0.29104845371857,
-0.903141581680914));
#21296=CARTESIAN_POINT('Ctrl Pts',(0.564362943424239,-0.28018331644634,
-0.916597376014514));
#21297=CARTESIAN_POINT('Ctrl Pts',(0.525933334162556,-0.254319232363049,
-0.939198248544427));
#21298=CARTESIAN_POINT('Ctrl Pts',(0.507057380724533,-0.237895043532788,
-0.949440676105255));
#21299=CARTESIAN_POINT('Ctrl Pts',(0.473077587363686,-0.199697230012983,
-0.966820759530997));
#21300=CARTESIAN_POINT('Ctrl Pts',(0.457978755888596,-0.177924977804098,
-0.973971221090534));
#21301=CARTESIAN_POINT('Ctrl Pts',(0.430199341854858,-0.124911173756694,
-0.986608710139579));
#21302=CARTESIAN_POINT('Ctrl Pts',(0.419070565453384,-0.0925528133349865,
-0.991263089003441));
#21303=CARTESIAN_POINT('Ctrl Pts',(0.413083465285518,-0.05953,-0.993751811093549));
#21304=CARTESIAN_POINT('Origin',(0.685838782044607,-0.05953,-0.860014630714833));
#21305=CARTESIAN_POINT('Origin',(0.,-0.208355,0.));
#21306=CARTESIAN_POINT('',(-1.076188,-0.35718,1.31795018948079E-16));
#21307=CARTESIAN_POINT('Origin',(0.,-0.35718,0.));
#21308=CARTESIAN_POINT('',(-1.076188,-0.208355,1.31795018948079E-16));
#21309=CARTESIAN_POINT('',(1.03449977959455,-0.05953,0.296632461748266));
#21310=CARTESIAN_POINT('Origin',(0.,-0.05953,0.));
#21311=CARTESIAN_POINT('',(1.03449977959455,-0.05953,-0.296632461748266));
#21312=CARTESIAN_POINT('Ctrl Pts',(1.03449977959455,-0.05953,0.296632461748267));
#21313=CARTESIAN_POINT('Ctrl Pts',(1.03628691421076,-0.0925528133349865,
0.290399865505497));
#21314=CARTESIAN_POINT('Ctrl Pts',(1.03958665287714,-0.124911173756694,
0.278797079997872));
#21315=CARTESIAN_POINT('Ctrl Pts',(1.0470264474309,-0.177924977804098,0.249198913998601));
#21316=CARTESIAN_POINT('Ctrl Pts',(1.05084995891418,-0.199697230012983,
0.232935932341942));
#21317=CARTESIAN_POINT('Ctrl Pts',(1.05844771715377,-0.237895043532788,
0.195533155353269));
#21318=CARTESIAN_POINT('Ctrl Pts',(1.06220882929878,-0.254319232363049,
0.17438929156337));
#21319=CARTESIAN_POINT('Ctrl Pts',(1.06849922508772,-0.28018331644634,0.130252399648131));
#21320=CARTESIAN_POINT('Ctrl Pts',(1.07137013248666,-0.29104845371857,0.105070977154072));
#21321=CARTESIAN_POINT('Ctrl Pts',(1.07522652957392,-0.30527573347708,0.0525526752791107));
#21322=CARTESIAN_POINT('Ctrl Pts',(1.076188,-0.308638795020976,0.025214283908933));
#21323=CARTESIAN_POINT('Ctrl Pts',(1.076188,-0.308638795020976,-0.025214283908933));
#21324=CARTESIAN_POINT('Ctrl Pts',(1.07522652957392,-0.30527573347708,-0.0525526752791107));
#21325=CARTESIAN_POINT('Ctrl Pts',(1.07137013248666,-0.29104845371857,-0.105070977154072));
#21326=CARTESIAN_POINT('Ctrl Pts',(1.06849922508772,-0.28018331644634,-0.130252399648131));
#21327=CARTESIAN_POINT('Ctrl Pts',(1.06220882929878,-0.254319232363049,
-0.17438929156337));
#21328=CARTESIAN_POINT('Ctrl Pts',(1.05844771715377,-0.237895043532788,
-0.195533155353269));
#21329=CARTESIAN_POINT('Ctrl Pts',(1.05084995891418,-0.199697230012983,
-0.232935932341942));
#21330=CARTESIAN_POINT('Ctrl Pts',(1.0470264474309,-0.177924977804098,-0.249198913998601));
#21331=CARTESIAN_POINT('Ctrl Pts',(1.03958665287714,-0.124911173756694,
-0.278797079997872));
#21332=CARTESIAN_POINT('Ctrl Pts',(1.03628691421076,-0.0925528133349865,
-0.290399865505497));
#21333=CARTESIAN_POINT('Ctrl Pts',(1.03449977959455,-0.05953,-0.296632461748267));
#21334=CARTESIAN_POINT('Origin',(0.,-0.05953,0.));
#21335=CARTESIAN_POINT('Origin',(0.,-0.05953,0.));
#21336=CARTESIAN_POINT('Origin',(1.1,-0.05953,0.));
#21337=CARTESIAN_POINT('Origin',(1.1,0.,0.));
#21338=CARTESIAN_POINT('Origin',(1.1,-0.05953,0.));
#21339=CARTESIAN_POINT('Origin',(0.,-0.35718,0.));
#21340=CARTESIAN_POINT('Origin',(0.,-0.05953,0.));
#21341=CARTESIAN_POINT('',(0.,0.,0.));
#21342=CARTESIAN_POINT('Origin',(1.119765,0.495,0.));
#21343=CARTESIAN_POINT('',(-1.119765,0.495,-1.37131662304724E-16));
#21344=CARTESIAN_POINT('Origin',(0.,0.495,0.));
#21345=CARTESIAN_POINT('',(-1.085235,0.495,-1.32902956907268E-16));
#21346=CARTESIAN_POINT('Origin',(0.,0.495,0.));
#21347=CARTESIAN_POINT('Origin',(0.,0.4575,0.));
#21348=CARTESIAN_POINT('',(-1.119765,0.42,-1.37131662304724E-16));
#21349=CARTESIAN_POINT('Origin',(0.,0.42,0.));
#21350=CARTESIAN_POINT('',(-1.119765,0.4575,-1.37131662304724E-16));
#21351=CARTESIAN_POINT('Origin',(1.085235,0.42,0.));
#21352=CARTESIAN_POINT('',(-1.085235,0.42,-1.32902956907268E-16));
#21353=CARTESIAN_POINT('Origin',(0.,0.42,0.));
#21354=CARTESIAN_POINT('Origin',(0.,0.4575,0.));
#21355=CARTESIAN_POINT('',(-1.085235,0.4575,-1.32902956907268E-16));
#21356=CARTESIAN_POINT('Origin',(1.119765,-0.42,0.));
#21357=CARTESIAN_POINT('',(-1.119765,-0.42,-1.37131662304724E-16));
#21358=CARTESIAN_POINT('Origin',(0.,-0.42,0.));
#21359=CARTESIAN_POINT('',(-1.085235,-0.42,-1.32902956907268E-16));
#21360=CARTESIAN_POINT('Origin',(0.,-0.42,0.));
#21361=CARTESIAN_POINT('Origin',(0.,-0.4575,0.));
#21362=CARTESIAN_POINT('',(-1.119765,-0.495,-1.37131662304724E-16));
#21363=CARTESIAN_POINT('Origin',(0.,-0.495,0.));
#21364=CARTESIAN_POINT('',(-1.119765,-0.4575,-1.37131662304724E-16));
#21365=CARTESIAN_POINT('Origin',(1.085235,-0.495,0.));
#21366=CARTESIAN_POINT('',(-1.085235,-0.495,-1.32902956907268E-16));
#21367=CARTESIAN_POINT('Origin',(0.,-0.495,0.));
#21368=CARTESIAN_POINT('Origin',(0.,-0.4575,0.));
#21369=CARTESIAN_POINT('',(-1.085235,-0.4575,-1.32902956907268E-16));
#21370=CARTESIAN_POINT('',(0.,0.,0.));
#21371=CARTESIAN_POINT('',(0.,0.,0.));
#21372=CARTESIAN_POINT('',(0.,0.,0.));
#21373=CARTESIAN_POINT('',(0.,0.,0.));
#21374=CARTESIAN_POINT('',(0.,0.,0.));
#21375=CARTESIAN_POINT('',(0.,0.,0.));
#21376=CARTESIAN_POINT('Origin',(0.0866025403784439,-0.4,-0.15));
#21377=CARTESIAN_POINT('',(0.173205080756888,-0.4,0.));
#21378=CARTESIAN_POINT('',(0.0866025403784439,-0.4,-0.15));
#21379=CARTESIAN_POINT('',(0.173205080756888,-0.4,0.));
#21380=CARTESIAN_POINT('',(0.0866025403784439,-0.64,-0.15));
#21381=CARTESIAN_POINT('',(0.0866025403784439,-0.4,-0.15));
#21382=CARTESIAN_POINT('',(0.173205080756888,-0.64,0.));
#21383=CARTESIAN_POINT('',(0.173205080756888,-0.64,0.));
#21384=CARTESIAN_POINT('',(0.173205080756888,-0.4,0.));
#21385=CARTESIAN_POINT('Origin',(-0.0866025403784438,-0.4,-0.15));
#21386=CARTESIAN_POINT('',(-0.0866025403784438,-0.4,-0.15));
#21387=CARTESIAN_POINT('',(0.0866025403784439,-0.4,-0.15));
#21388=CARTESIAN_POINT('',(-0.0866025403784438,-0.64,-0.15));
#21389=CARTESIAN_POINT('',(-0.0866025403784438,-0.4,-0.15));
#21390=CARTESIAN_POINT('',(0.0866025403784439,-0.64,-0.15));
#21391=CARTESIAN_POINT('Origin',(-0.173205080756888,-0.4,-2.77555756156289E-17));
#21392=CARTESIAN_POINT('',(-0.173205080756888,-0.4,-2.12115047744981E-17));
#21393=CARTESIAN_POINT('',(-0.0866025403784438,-0.4,-0.15));
#21394=CARTESIAN_POINT('',(-0.173205080756888,-0.64,-2.77555756156289E-17));
#21395=CARTESIAN_POINT('',(-0.173205080756888,-0.4,-2.12115047744981E-17));
#21396=CARTESIAN_POINT('',(-0.0866025403784438,-0.64,-0.15));
#21397=CARTESIAN_POINT('Origin',(-0.0866025403784439,-0.4,0.15));
#21398=CARTESIAN_POINT('',(-0.0866025403784439,-0.4,0.15));
#21399=CARTESIAN_POINT('',(-0.173205080756888,-0.4,-2.12115047744981E-17));
#21400=CARTESIAN_POINT('',(-0.0866025403784439,-0.64,0.15));
#21401=CARTESIAN_POINT('',(-0.0866025403784439,-0.4,0.15));
#21402=CARTESIAN_POINT('',(-0.173205080756888,-0.64,-2.12115047744981E-17));
#21403=CARTESIAN_POINT('Origin',(0.0866025403784439,-0.4,0.15));
#21404=CARTESIAN_POINT('',(0.0866025403784439,-0.4,0.15));
#21405=CARTESIAN_POINT('',(-0.0866025403784439,-0.4,0.15));
#21406=CARTESIAN_POINT('',(0.0866025403784439,-0.64,0.15));
#21407=CARTESIAN_POINT('',(0.0866025403784439,-0.4,0.15));
#21408=CARTESIAN_POINT('',(-0.0866025403784439,-0.64,0.15));
#21409=CARTESIAN_POINT('Origin',(0.173205080756888,-0.4,0.));
#21410=CARTESIAN_POINT('',(0.0866025403784439,-0.4,0.15));
#21411=CARTESIAN_POINT('',(0.0866025403784439,-0.64,0.15));
#21412=CARTESIAN_POINT('Origin',(0.,-0.4,-2.77555756156289E-17));
#21413=CARTESIAN_POINT('Origin',(0.,-0.64,-2.77555756156289E-17));
#21414=CARTESIAN_POINT('Origin',(0.,-1.,0.));
#21415=CARTESIAN_POINT('',(-0.1954,-1.,2.39295984553393E-17));
#21416=CARTESIAN_POINT('Origin',(0.,-1.,0.));
#21417=CARTESIAN_POINT('Origin',(0.3,0.4,0.));
#21418=CARTESIAN_POINT('',(-0.3,0.4,-3.67394039744206E-17));
#21419=CARTESIAN_POINT('Origin',(0.,0.4,0.));
#21420=CARTESIAN_POINT('Origin',(0.,0.375,0.));
#21421=CARTESIAN_POINT('',(-0.35,0.35,-4.28626379701573E-17));
#21422=CARTESIAN_POINT('Origin',(0.,0.35,0.));
#21423=CARTESIAN_POINT('',(-0.325,0.375,-3.9801020972289E-17));
#21424=CARTESIAN_POINT('Origin',(0.,0.19,0.));
#21425=CARTESIAN_POINT('',(-0.35,0.03,-4.28626379701574E-17));
#21426=CARTESIAN_POINT('Origin',(0.,0.03,0.));
#21427=CARTESIAN_POINT('',(-0.35,0.19,-4.28626379701574E-17));
#21428=CARTESIAN_POINT('Origin',(0.,0.0149999999999999,0.));
#21429=CARTESIAN_POINT('',(-0.32,-3.29597460435593E-17,-3.91886975727153E-17));
#21430=CARTESIAN_POINT('Origin',(0.,0.,0.));
#21431=CARTESIAN_POINT('',(-0.335,0.0149999999999999,-4.10256677714363E-17));
#21432=CARTESIAN_POINT('Origin',(0.22,0.,0.));
#21433=CARTESIAN_POINT('',(-0.22,-6.93889390390723E-18,-2.69422295812418E-17));
#21434=CARTESIAN_POINT('Origin',(0.,0.,0.));
#21435=CARTESIAN_POINT('Origin',(0.,-0.02,0.));
#21436=CARTESIAN_POINT('',(-0.1954,-0.0492,2.39295984553393E-17));
#21437=CARTESIAN_POINT('Origin',(0.,-0.0492,0.));
#21438=CARTESIAN_POINT('',(-0.21,-0.02,-2.57175827820944E-17));
#21439=CARTESIAN_POINT('Origin',(0.,-0.8,0.));
#21440=CARTESIAN_POINT('',(-0.1954,-0.8,-2.39295984553393E-17));
#21441=CARTESIAN_POINT('',(0.,0.,0.));
#21442=CARTESIAN_POINT('',(0.,0.,0.));
#21443=CARTESIAN_POINT('Origin',(0.,-5.1,7.));
#21444=CARTESIAN_POINT('',(-0.165,-5.,7.));
#21445=CARTESIAN_POINT('Origin',(0.,-5.,7.));
#21446=CARTESIAN_POINT('',(-0.165,-3.4,7.));
#21447=CARTESIAN_POINT('',(-0.165,-5.1,7.));
#21448=CARTESIAN_POINT('Origin',(0.,-3.4,7.));
#21449=CARTESIAN_POINT('Origin',(0.,-3.4,7.));
#21450=CARTESIAN_POINT('Origin',(0.,2.05,7.));
#21451=CARTESIAN_POINT('',(-0.7,2.05,7.));
#21452=CARTESIAN_POINT('Origin',(0.,2.05,7.));
#21453=CARTESIAN_POINT('',(-0.5,2.05,7.));
#21454=CARTESIAN_POINT('Origin',(0.,2.05,7.));
#21455=CARTESIAN_POINT('Origin',(0.,1.35,7.));
#21456=CARTESIAN_POINT('',(-0.7,1.35,7.));
#21457=CARTESIAN_POINT('Origin',(0.,1.35,7.));
#21458=CARTESIAN_POINT('',(-0.5,1.35,7.));
#21459=CARTESIAN_POINT('Origin',(0.,1.35,7.));
#21460=CARTESIAN_POINT('Origin',(0.,1.35,7.));
#21461=CARTESIAN_POINT('',(-0.7,1.35,7.));
#21462=CARTESIAN_POINT('Origin',(0.,-1.8,7.));
#21463=CARTESIAN_POINT('',(-0.5,-1.8,7.));
#21464=CARTESIAN_POINT('',(-0.5,-1.8,7.));
#21465=CARTESIAN_POINT('Origin',(0.,-1.8,7.));
#21466=CARTESIAN_POINT('Origin',(0.,-5.,7.));
#21467=CARTESIAN_POINT('',(-0.4,-1.8,7.));
#21468=CARTESIAN_POINT('Origin',(0.,-1.8,7.));
#21469=CARTESIAN_POINT('',(-0.4,-5.,7.));
#21470=CARTESIAN_POINT('',(-0.4,-5.,7.));
#21471=CARTESIAN_POINT('Origin',(0.,-5.,7.));
#21472=CARTESIAN_POINT('Origin',(0.,-5.,7.));
#21473=CARTESIAN_POINT('Origin',(0.,-1.8,7.));
#21474=CARTESIAN_POINT('',(-0.5,3.,7.));
#21475=CARTESIAN_POINT('Origin',(0.,3.,7.));
#21476=CARTESIAN_POINT('',(-0.5,-1.8,7.));
#21477=CARTESIAN_POINT('Origin',(0.,3.,7.));
#21478=CARTESIAN_POINT('Origin',(0.,-1.8,7.));
#21479=CARTESIAN_POINT('',(0.,0.,0.));
#21480=CARTESIAN_POINT('Origin',(0.,-1.8,7.));
#21481=CARTESIAN_POINT('',(-0.505,-1.8,7.));
#21482=CARTESIAN_POINT('Origin',(0.,-1.8,7.));
#21483=CARTESIAN_POINT('',(-0.505,-1.35,7.));
#21484=CARTESIAN_POINT('',(-0.505,-1.8,7.));
#21485=CARTESIAN_POINT('Origin',(0.,-1.35,7.));
#21486=CARTESIAN_POINT('Origin',(0.,-1.8,7.));
#21487=CARTESIAN_POINT('',(-0.405,-1.8,7.));
#21488=CARTESIAN_POINT('Origin',(0.,-1.8,7.));
#21489=CARTESIAN_POINT('Origin',(0.,-2.65,7.));
#21490=CARTESIAN_POINT('',(-0.405,-2.65,7.));
#21491=CARTESIAN_POINT('',(-0.405,-2.65,7.));
#21492=CARTESIAN_POINT('Origin',(0.,-2.65,7.));
#21493=CARTESIAN_POINT('Origin',(0.,-2.65,7.));
#21494=CARTESIAN_POINT('',(-0.7,-1.35,7.));
#21495=CARTESIAN_POINT('Origin',(0.,-1.35,7.));
#21496=CARTESIAN_POINT('',(-0.7,-2.65,7.));
#21497=CARTESIAN_POINT('',(-0.7,-2.65,7.));
#21498=CARTESIAN_POINT('Origin',(0.,-2.65,7.));
#21499=CARTESIAN_POINT('Origin',(0.,-1.35,7.));
#21500=CARTESIAN_POINT('Origin',(0.,-2.65,7.));
#21501=CARTESIAN_POINT('',(0.,0.,0.));
#21502=CARTESIAN_POINT('Origin',(0.,-0.45,7.));
#21503=CARTESIAN_POINT('',(-0.505,0.45,7.));
#21504=CARTESIAN_POINT('Origin',(0.,0.45,7.));
#21505=CARTESIAN_POINT('',(-0.505,-0.45,7.));
#21506=CARTESIAN_POINT('',(-0.505,-0.45,7.));
#21507=CARTESIAN_POINT('Origin',(0.,-0.45,7.));
#21508=CARTESIAN_POINT('Origin',(0.,-0.45,7.));
#21509=CARTESIAN_POINT('',(-0.7,0.45,7.));
#21510=CARTESIAN_POINT('Origin',(0.,0.45,7.));
#21511=CARTESIAN_POINT('',(-0.7,-0.45,7.));
#21512=CARTESIAN_POINT('',(-0.7,-0.45,7.));
#21513=CARTESIAN_POINT('Origin',(0.,-0.45,7.));
#21514=CARTESIAN_POINT('Origin',(0.,0.45,7.));
#21515=CARTESIAN_POINT('Origin',(0.,-0.45,7.));
#21516=CARTESIAN_POINT('',(0.,0.,0.));
#21517=CARTESIAN_POINT('Origin',(0.,-3.95,6.35));
#21518=CARTESIAN_POINT('',(-0.15,-3.95,6.6));
#21519=CARTESIAN_POINT('Origin',(0.,-3.95,6.6));
#21520=CARTESIAN_POINT('',(-0.15,-3.95,6.35));
#21521=CARTESIAN_POINT('',(-0.15,-3.95,6.35));
#21522=CARTESIAN_POINT('Origin',(0.,-3.95,6.35));
#21523=CARTESIAN_POINT('Origin',(0.,-3.95,6.6));
#21524=CARTESIAN_POINT('Origin',(0.,-3.95,6.35));
#21525=CARTESIAN_POINT('',(0.,0.,0.));
#21526=CARTESIAN_POINT('Origin',(0.,-3.95,7.4));
#21527=CARTESIAN_POINT('',(-0.15,-3.95,7.65));
#21528=CARTESIAN_POINT('Origin',(0.,-3.95,7.65));
#21529=CARTESIAN_POINT('',(-0.15,-3.95,7.4));
#21530=CARTESIAN_POINT('',(-0.15,-3.95,7.4));
#21531=CARTESIAN_POINT('Origin',(0.,-3.95,7.4));
#21532=CARTESIAN_POINT('Origin',(0.,-3.95,7.65));
#21533=CARTESIAN_POINT('Origin',(0.,-3.95,7.4));
#21534=CARTESIAN_POINT('',(0.,0.,0.));
#21535=CARTESIAN_POINT('Origin',(0.,-5.2,7.));
#21536=CARTESIAN_POINT('',(-0.225,-5.,7.));
#21537=CARTESIAN_POINT('Origin',(0.,-5.,7.));
#21538=CARTESIAN_POINT('',(-0.225,-5.2,7.));
#21539=CARTESIAN_POINT('',(-0.225,-5.2,7.));
#21540=CARTESIAN_POINT('Origin',(0.,-5.2,7.));
#21541=CARTESIAN_POINT('Origin',(0.,-5.2,7.));
#21542=CARTESIAN_POINT('',(-0.6,-5.,7.));
#21543=CARTESIAN_POINT('Origin',(0.,-5.,7.));
#21544=CARTESIAN_POINT('',(-0.6,-5.2,7.));
#21545=CARTESIAN_POINT('',(-0.6,-5.2,7.));
#21546=CARTESIAN_POINT('Origin',(0.,-5.2,7.));
#21547=CARTESIAN_POINT('Origin',(0.,-5.,7.));
#21548=CARTESIAN_POINT('Origin',(0.,-5.2,7.));
#21549=CARTESIAN_POINT('',(0.,0.,0.));
#21550=CARTESIAN_POINT('Origin',(0.,-0.45,0.));
#21551=CARTESIAN_POINT('',(-0.65,-0.325,-3.9801020972289E-17));
#21552=CARTESIAN_POINT('',(-0.637867541108654,-0.45,0.125));
#21553=CARTESIAN_POINT('Ctrl Pts',(-0.65,-0.325,-6.93889390390723E-17));
#21554=CARTESIAN_POINT('Ctrl Pts',(-0.65,-0.325,0.0157371373481997));
#21555=CARTESIAN_POINT('Ctrl Pts',(-0.649370620646074,-0.328153081062251,
0.0324967135411163));
#21556=CARTESIAN_POINT('Ctrl Pts',(-0.647096224417991,-0.340922081922822,
0.0632828231545122));
#21557=CARTESIAN_POINT('Ctrl Pts',(-0.645482573914132,-0.350535859112198,
0.0773125544088347));
#21558=CARTESIAN_POINT('Ctrl Pts',(-0.642442040715078,-0.372687974598127,
0.0994646698947638));
#21559=CARTESIAN_POINT('Ctrl Pts',(-0.640815160902589,-0.386717480603274,
0.109078032552995));
#21560=CARTESIAN_POINT('Ctrl Pts',(-0.63851034608138,-0.417502809542363,
0.121846732641678));
#21561=CARTESIAN_POINT('Ctrl Pts',(-0.637867541108654,-0.434262111007648,
0.125));
#21562=CARTESIAN_POINT('Ctrl Pts',(-0.637867541108654,-0.45,0.125));
#21563=CARTESIAN_POINT('',(-0.65,-0.575,-3.9801020972289E-17));
#21564=CARTESIAN_POINT('Ctrl Pts',(-0.65,-0.575,-3.46944695195361E-18));
#21565=CARTESIAN_POINT('Ctrl Pts',(-0.65,-0.575,-0.0157371373481998));
#21566=CARTESIAN_POINT('Ctrl Pts',(-0.649370620646074,-0.571846918937749,
-0.0324967135411164));
#21567=CARTESIAN_POINT('Ctrl Pts',(-0.647096224417991,-0.559077918077178,
-0.0632828231545123));
#21568=CARTESIAN_POINT('Ctrl Pts',(-0.645482573914132,-0.549464140887802,
-0.0773125544088349));
#21569=CARTESIAN_POINT('Ctrl Pts',(-0.642442040715078,-0.527312025401873,
-0.099464669894764));
#21570=CARTESIAN_POINT('Ctrl Pts',(-0.640815160902589,-0.513282519396725,
-0.109078032552995));
#21571=CARTESIAN_POINT('Ctrl Pts',(-0.63851034608138,-0.482497190457637,
-0.121846732641678));
#21572=CARTESIAN_POINT('Ctrl Pts',(-0.637867541108654,-0.465737888992352,
-0.125));
#21573=CARTESIAN_POINT('Ctrl Pts',(-0.637867541108654,-0.434262111007648,
-0.125));
#21574=CARTESIAN_POINT('Ctrl Pts',(-0.63851034608138,-0.417502809542363,
-0.121846732641678));
#21575=CARTESIAN_POINT('Ctrl Pts',(-0.640815160902589,-0.386717480603275,
-0.109078032552995));
#21576=CARTESIAN_POINT('Ctrl Pts',(-0.642442040715078,-0.372687974598127,
-0.099464669894764));
#21577=CARTESIAN_POINT('Ctrl Pts',(-0.645482573914132,-0.350535859112198,
-0.077312554408835));
#21578=CARTESIAN_POINT('Ctrl Pts',(-0.647096224417991,-0.340922081922822,
-0.0632828231545124));
#21579=CARTESIAN_POINT('Ctrl Pts',(-0.649370620646074,-0.328153081062251,
-0.0324967135411165));
#21580=CARTESIAN_POINT('Ctrl Pts',(-0.65,-0.325,-0.0157371373481999));
#21581=CARTESIAN_POINT('Ctrl Pts',(-0.65,-0.325,-8.32667268468867E-17));
#21582=CARTESIAN_POINT('Ctrl Pts',(-0.637867541108654,-0.45,0.125));
#21583=CARTESIAN_POINT('Ctrl Pts',(-0.637867541108654,-0.465737888992352,
0.125));
#21584=CARTESIAN_POINT('Ctrl Pts',(-0.63851034608138,-0.482497190457637,
0.121846732641678));
#21585=CARTESIAN_POINT('Ctrl Pts',(-0.640815160902589,-0.513282519396725,
0.109078032552995));
#21586=CARTESIAN_POINT('Ctrl Pts',(-0.642442040715078,-0.527312025401873,
0.0994646698947639));
#21587=CARTESIAN_POINT('Ctrl Pts',(-0.645482573914132,-0.549464140887802,
0.0773125544088349));
#21588=CARTESIAN_POINT('Ctrl Pts',(-0.647096224417991,-0.559077918077178,
0.0632828231545123));
#21589=CARTESIAN_POINT('Ctrl Pts',(-0.649370620646074,-0.571846918937749,
0.0324967135411164));
#21590=CARTESIAN_POINT('Ctrl Pts',(-0.65,-0.575,0.0157371373481998));
#21591=CARTESIAN_POINT('Ctrl Pts',(-0.65,-0.575,-2.08166817117217E-17));
#21592=CARTESIAN_POINT('',(-0.379967103839267,-0.45,0.125));
#21593=CARTESIAN_POINT('',(-7.65404249467096E-18,-0.45,0.125));
#21594=CARTESIAN_POINT('',(-0.4,-0.575,5.41097774720219E-18));
#21595=CARTESIAN_POINT('Ctrl Pts',(-0.4,-0.575,-3.81639164714898E-17));
#21596=CARTESIAN_POINT('Ctrl Pts',(-0.4,-0.575,0.0158075115832675));
#21597=CARTESIAN_POINT('Ctrl Pts',(-0.398970551469948,-0.571819306519379,
0.0325978607437828));
#21598=CARTESIAN_POINT('Ctrl Pts',(-0.395252954914593,-0.559029081159106,
0.0633657881355917));
#21599=CARTESIAN_POINT('Ctrl Pts',(-0.392612801026882,-0.549425200318011,
0.0773514949786256));
#21600=CARTESIAN_POINT('Ctrl Pts',(-0.38761064154154,-0.527347592689753,
0.0994291026068839));
#21601=CARTESIAN_POINT('Ctrl Pts',(-0.384911758361269,-0.51336346023721,
0.109029967924066));
#21602=CARTESIAN_POINT('Ctrl Pts',(-0.381057715344782,-0.48260129709332,
0.121817958968287));
#21603=CARTESIAN_POINT('Ctrl Pts',(-0.379967103839267,-0.465813100629203,
0.125));
#21604=CARTESIAN_POINT('Ctrl Pts',(-0.379967103839267,-0.45,0.125));
#21605=CARTESIAN_POINT('',(-0.379967103839267,-0.45,-0.125));
#21606=CARTESIAN_POINT('Ctrl Pts',(-0.379967103839267,-0.45,-0.125));
#21607=CARTESIAN_POINT('Ctrl Pts',(-0.379967103839267,-0.465813100629203,
-0.125));
#21608=CARTESIAN_POINT('Ctrl Pts',(-0.381057715344782,-0.48260129709332,
-0.121817958968287));
#21609=CARTESIAN_POINT('Ctrl Pts',(-0.384911758361269,-0.51336346023721,
-0.109029967924066));
#21610=CARTESIAN_POINT('Ctrl Pts',(-0.38761064154154,-0.527347592689753,
-0.099429102606884));
#21611=CARTESIAN_POINT('Ctrl Pts',(-0.392612801026882,-0.549425200318011,
-0.0773514949786257));
#21612=CARTESIAN_POINT('Ctrl Pts',(-0.395252954914593,-0.559029081159106,
-0.0633657881355918));
#21613=CARTESIAN_POINT('Ctrl Pts',(-0.398970551469948,-0.571819306519379,
-0.0325978607437828));
#21614=CARTESIAN_POINT('Ctrl Pts',(-0.4,-0.575,-0.0158075115832676));
#21615=CARTESIAN_POINT('Ctrl Pts',(-0.4,-0.575,-4.16333634234434E-17));
#21616=CARTESIAN_POINT('',(-0.4,-0.325,2.96971064108775E-17));
#21617=CARTESIAN_POINT('Ctrl Pts',(-0.4,-0.325,1.04083408558608E-17));
#21618=CARTESIAN_POINT('Ctrl Pts',(-0.4,-0.325,-0.0158075115832676));
#21619=CARTESIAN_POINT('Ctrl Pts',(-0.398970551469948,-0.328180693480621,
-0.0325978607437828));
#21620=CARTESIAN_POINT('Ctrl Pts',(-0.395252954914593,-0.340970918840894,
-0.0633657881355918));
#21621=CARTESIAN_POINT('Ctrl Pts',(-0.392612801026882,-0.350574799681989,
-0.0773514949786256));
#21622=CARTESIAN_POINT('Ctrl Pts',(-0.38761064154154,-0.372652407310247,
-0.0994291026068839));
#21623=CARTESIAN_POINT('Ctrl Pts',(-0.384911758361269,-0.38663653976279,
-0.109029967924066));
#21624=CARTESIAN_POINT('Ctrl Pts',(-0.381057715344782,-0.41739870290668,
-0.121817958968287));
#21625=CARTESIAN_POINT('Ctrl Pts',(-0.379967103839267,-0.434186899370797,
-0.125));
#21626=CARTESIAN_POINT('Ctrl Pts',(-0.379967103839267,-0.45,-0.125));
#21627=CARTESIAN_POINT('Ctrl Pts',(-0.379967103839267,-0.45,0.125));
#21628=CARTESIAN_POINT('Ctrl Pts',(-0.379967103839267,-0.434186899370797,
0.125));
#21629=CARTESIAN_POINT('Ctrl Pts',(-0.381057715344782,-0.41739870290668,
0.121817958968287));
#21630=CARTESIAN_POINT('Ctrl Pts',(-0.384911758361269,-0.38663653976279,
0.109029967924066));
#21631=CARTESIAN_POINT('Ctrl Pts',(-0.38761064154154,-0.372652407310247,
0.0994291026068839));
#21632=CARTESIAN_POINT('Ctrl Pts',(-0.392612801026882,-0.350574799681989,
0.0773514949786257));
#21633=CARTESIAN_POINT('Ctrl Pts',(-0.395252954914593,-0.340970918840894,
0.0633657881355918));
#21634=CARTESIAN_POINT('Ctrl Pts',(-0.398970551469948,-0.328180693480621,
0.0325978607437829));
#21635=CARTESIAN_POINT('Ctrl Pts',(-0.4,-0.325,0.0158075115832676));
#21636=CARTESIAN_POINT('Ctrl Pts',(-0.4,-0.325,1.38777878078145E-17));
#21637=CARTESIAN_POINT('Origin',(0.,-0.45,0.));
#21638=CARTESIAN_POINT('',(0.379967103839267,-0.45,-0.125));
#21639=CARTESIAN_POINT('',(0.379967103839267,-0.45,0.125));
#21640=CARTESIAN_POINT('Ctrl Pts',(0.379967103839267,-0.45,-0.125));
#21641=CARTESIAN_POINT('Ctrl Pts',(0.379967103839267,-0.434186899370797,
-0.125));
#21642=CARTESIAN_POINT('Ctrl Pts',(0.381057715344782,-0.41739870290668,
-0.121817958968287));
#21643=CARTESIAN_POINT('Ctrl Pts',(0.384911758361269,-0.38663653976279,
-0.109029967924066));
#21644=CARTESIAN_POINT('Ctrl Pts',(0.38761064154154,-0.372652407310247,
-0.0994291026068839));
#21645=CARTESIAN_POINT('Ctrl Pts',(0.392612801026882,-0.350574799681989,
-0.0773514949786256));
#21646=CARTESIAN_POINT('Ctrl Pts',(0.395252954914593,-0.340970918840894,
-0.0633657881355917));
#21647=CARTESIAN_POINT('Ctrl Pts',(0.398970551469948,-0.328180693480621,
-0.0325978607437828));
#21648=CARTESIAN_POINT('Ctrl Pts',(0.4,-0.325,-0.0158075115832675));
#21649=CARTESIAN_POINT('Ctrl Pts',(0.4,-0.325,0.0158075115832676));
#21650=CARTESIAN_POINT('Ctrl Pts',(0.398970551469948,-0.328180693480621,
0.0325978607437829));
#21651=CARTESIAN_POINT('Ctrl Pts',(0.395252954914593,-0.340970918840894,
0.0633657881355918));
#21652=CARTESIAN_POINT('Ctrl Pts',(0.392612801026882,-0.350574799681989,
0.0773514949786257));
#21653=CARTESIAN_POINT('Ctrl Pts',(0.38761064154154,-0.372652407310247,
0.099429102606884));
#21654=CARTESIAN_POINT('Ctrl Pts',(0.384911758361269,-0.38663653976279,
0.109029967924066));
#21655=CARTESIAN_POINT('Ctrl Pts',(0.381057715344782,-0.41739870290668,
0.121817958968287));
#21656=CARTESIAN_POINT('Ctrl Pts',(0.379967103839267,-0.434186899370797,
0.125));
#21657=CARTESIAN_POINT('Ctrl Pts',(0.379967103839267,-0.45,0.125));
#21658=CARTESIAN_POINT('Ctrl Pts',(0.379967103839267,-0.45,0.125));
#21659=CARTESIAN_POINT('Ctrl Pts',(0.379967103839267,-0.465813100629203,
0.125));
#21660=CARTESIAN_POINT('Ctrl Pts',(0.381057715344782,-0.48260129709332,
0.121817958968287));
#21661=CARTESIAN_POINT('Ctrl Pts',(0.384911758361269,-0.51336346023721,
0.109029967924066));
#21662=CARTESIAN_POINT('Ctrl Pts',(0.38761064154154,-0.527347592689753,
0.0994291026068839));
#21663=CARTESIAN_POINT('Ctrl Pts',(0.392612801026882,-0.549425200318011,
0.0773514949786257));
#21664=CARTESIAN_POINT('Ctrl Pts',(0.395252954914593,-0.559029081159106,
0.0633657881355918));
#21665=CARTESIAN_POINT('Ctrl Pts',(0.398970551469948,-0.571819306519379,
0.0325978607437829));
#21666=CARTESIAN_POINT('Ctrl Pts',(0.4,-0.575,0.0158075115832676));
#21667=CARTESIAN_POINT('Ctrl Pts',(0.4,-0.575,-0.0158075115832676));
#21668=CARTESIAN_POINT('Ctrl Pts',(0.398970551469948,-0.57181930651938,
-0.0325978607437828));
#21669=CARTESIAN_POINT('Ctrl Pts',(0.395252954914593,-0.559029081159106,
-0.0633657881355918));
#21670=CARTESIAN_POINT('Ctrl Pts',(0.392612801026882,-0.549425200318011,
-0.0773514949786257));
#21671=CARTESIAN_POINT('Ctrl Pts',(0.38761064154154,-0.527347592689753,
-0.0994291026068839));
#21672=CARTESIAN_POINT('Ctrl Pts',(0.384911758361269,-0.51336346023721,
-0.109029967924066));
#21673=CARTESIAN_POINT('Ctrl Pts',(0.381057715344782,-0.48260129709332,
-0.121817958968287));
#21674=CARTESIAN_POINT('Ctrl Pts',(0.379967103839267,-0.465813100629203,
-0.125));
#21675=CARTESIAN_POINT('Ctrl Pts',(0.379967103839267,-0.45,-0.125));
#21676=CARTESIAN_POINT('',(0.637867541108654,-0.45,0.125));
#21677=CARTESIAN_POINT('',(-7.65404249467096E-18,-0.45,0.125));
#21678=CARTESIAN_POINT('',(0.65,-0.575,3.9801020972289E-17));
#21679=CARTESIAN_POINT('Ctrl Pts',(0.65,-0.575,5.55111512312578E-17));
#21680=CARTESIAN_POINT('Ctrl Pts',(0.65,-0.575,0.0157371373481999));
#21681=CARTESIAN_POINT('Ctrl Pts',(0.649370620646074,-0.571846918937749,
0.0324967135411165));
#21682=CARTESIAN_POINT('Ctrl Pts',(0.647096224417991,-0.559077918077178,
0.0632828231545124));
#21683=CARTESIAN_POINT('Ctrl Pts',(0.645482573914132,-0.549464140887802,
0.077312554408835));
#21684=CARTESIAN_POINT('Ctrl Pts',(0.642442040715078,-0.527312025401873,
0.099464669894764));
#21685=CARTESIAN_POINT('Ctrl Pts',(0.640815160902589,-0.513282519396725,
0.109078032552995));
#21686=CARTESIAN_POINT('Ctrl Pts',(0.63851034608138,-0.482497190457637,
0.121846732641678));
#21687=CARTESIAN_POINT('Ctrl Pts',(0.637867541108654,-0.465737888992352,
0.125));
#21688=CARTESIAN_POINT('Ctrl Pts',(0.637867541108654,-0.45,0.125));
#21689=CARTESIAN_POINT('',(0.65,-0.325,3.9801020972289E-17));
#21690=CARTESIAN_POINT('Ctrl Pts',(0.65,-0.325,6.93889390390723E-18));
#21691=CARTESIAN_POINT('Ctrl Pts',(0.65,-0.325,-0.0157371373481998));
#21692=CARTESIAN_POINT('Ctrl Pts',(0.649370620646074,-0.328153081062251,
-0.0324967135411164));
#21693=CARTESIAN_POINT('Ctrl Pts',(0.647096224417991,-0.340922081922822,
-0.0632828231545123));
#21694=CARTESIAN_POINT('Ctrl Pts',(0.645482573914132,-0.350535859112198,
-0.0773125544088349));
#21695=CARTESIAN_POINT('Ctrl Pts',(0.642442040715078,-0.372687974598127,
-0.0994646698947639));
#21696=CARTESIAN_POINT('Ctrl Pts',(0.640815160902588,-0.386717480603275,
-0.109078032552995));
#21697=CARTESIAN_POINT('Ctrl Pts',(0.63851034608138,-0.417502809542363,
-0.121846732641678));
#21698=CARTESIAN_POINT('Ctrl Pts',(0.637867541108654,-0.434262111007648,
-0.125));
#21699=CARTESIAN_POINT('Ctrl Pts',(0.637867541108654,-0.465737888992352,
-0.125));
#21700=CARTESIAN_POINT('Ctrl Pts',(0.63851034608138,-0.482497190457637,
-0.121846732641678));
#21701=CARTESIAN_POINT('Ctrl Pts',(0.640815160902589,-0.513282519396725,
-0.109078032552995));
#21702=CARTESIAN_POINT('Ctrl Pts',(0.642442040715078,-0.527312025401873,
-0.0994646698947639));
#21703=CARTESIAN_POINT('Ctrl Pts',(0.645482573914132,-0.549464140887802,
-0.0773125544088348));
#21704=CARTESIAN_POINT('Ctrl Pts',(0.647096224417991,-0.559077918077178,
-0.0632828231545123));
#21705=CARTESIAN_POINT('Ctrl Pts',(0.649370620646074,-0.571846918937749,
-0.0324967135411164));
#21706=CARTESIAN_POINT('Ctrl Pts',(0.65,-0.575,-0.0157371373481998));
#21707=CARTESIAN_POINT('Ctrl Pts',(0.65,-0.575,6.24500451351651E-17));
#21708=CARTESIAN_POINT('Ctrl Pts',(0.637867541108654,-0.45,0.125));
#21709=CARTESIAN_POINT('Ctrl Pts',(0.637867541108654,-0.434262111007648,
0.125));
#21710=CARTESIAN_POINT('Ctrl Pts',(0.63851034608138,-0.417502809542363,
0.121846732641678));
#21711=CARTESIAN_POINT('Ctrl Pts',(0.640815160902589,-0.386717480603274,
0.109078032552995));
#21712=CARTESIAN_POINT('Ctrl Pts',(0.642442040715078,-0.372687974598127,
0.0994646698947639));
#21713=CARTESIAN_POINT('Ctrl Pts',(0.645482573914132,-0.350535859112198,
0.0773125544088348));
#21714=CARTESIAN_POINT('Ctrl Pts',(0.647096224417991,-0.340922081922822,
0.0632828231545123));
#21715=CARTESIAN_POINT('Ctrl Pts',(0.649370620646074,-0.328153081062251,
0.0324967135411164));
#21716=CARTESIAN_POINT('Ctrl Pts',(0.65,-0.325,0.0157371373481998));
#21717=CARTESIAN_POINT('Ctrl Pts',(0.65,-0.325,-6.93889390390723E-18));
#21718=CARTESIAN_POINT('Origin',(0.,-0.1,0.));
#21719=CARTESIAN_POINT('',(-0.65,-0.8,7.9602041944578E-17));
#21720=CARTESIAN_POINT('Origin',(0.,-0.8,0.));
#21721=CARTESIAN_POINT('',(-0.65,-0.1,-7.9602041944578E-17));
#21722=CARTESIAN_POINT('',(-0.65,-0.1,7.9602041944578E-17));
#21723=CARTESIAN_POINT('',(-0.65,-0.1,-7.9602041944578E-17));
#21724=CARTESIAN_POINT('Origin',(0.,-0.1,0.));
#21725=CARTESIAN_POINT('',(0.,-0.575,-0.65));
#21726=CARTESIAN_POINT('',(0.,-0.325,-0.65));
#21727=CARTESIAN_POINT('Ctrl Pts',(-1.73472347597681E-17,-0.575,-0.65));
#21728=CARTESIAN_POINT('Ctrl Pts',(0.0157371373481998,-0.575,-0.65));
#21729=CARTESIAN_POINT('Ctrl Pts',(0.0324967135411164,-0.571846918937749,
-0.649370620646074));
#21730=CARTESIAN_POINT('Ctrl Pts',(0.0632828231545123,-0.559077918077178,
-0.647096224417991));
#21731=CARTESIAN_POINT('Ctrl Pts',(0.0773125544088349,-0.549464140887802,
-0.645482573914132));
#21732=CARTESIAN_POINT('Ctrl Pts',(0.099464669894764,-0.527312025401873,
-0.642442040715078));
#21733=CARTESIAN_POINT('Ctrl Pts',(0.109078032552995,-0.513282519396725,
-0.640815160902589));
#21734=CARTESIAN_POINT('Ctrl Pts',(0.121846732641678,-0.482497190457636,
-0.63851034608138));
#21735=CARTESIAN_POINT('Ctrl Pts',(0.125,-0.465737888992352,-0.637867541108654));
#21736=CARTESIAN_POINT('Ctrl Pts',(0.125,-0.434262111007648,-0.637867541108654));
#21737=CARTESIAN_POINT('Ctrl Pts',(0.121846732641678,-0.417502809542364,
-0.63851034608138));
#21738=CARTESIAN_POINT('Ctrl Pts',(0.109078032552995,-0.386717480603275,
-0.640815160902589));
#21739=CARTESIAN_POINT('Ctrl Pts',(0.099464669894764,-0.372687974598127,
-0.642442040715078));
#21740=CARTESIAN_POINT('Ctrl Pts',(0.0773125544088349,-0.350535859112198,
-0.645482573914132));
#21741=CARTESIAN_POINT('Ctrl Pts',(0.0632828231545123,-0.340922081922822,
-0.647096224417991));
#21742=CARTESIAN_POINT('Ctrl Pts',(0.0324967135411164,-0.328153081062251,
-0.649370620646074));
#21743=CARTESIAN_POINT('Ctrl Pts',(0.0157371373481999,-0.325,-0.65));
#21744=CARTESIAN_POINT('Ctrl Pts',(4.5102810375397E-17,-0.325,-0.65));
#21745=CARTESIAN_POINT('',(-0.125,-0.45,-0.637867541108654));
#21746=CARTESIAN_POINT('Ctrl Pts',(4.85722573273506E-17,-0.325,-0.65));
#21747=CARTESIAN_POINT('Ctrl Pts',(-0.0157371373481997,-0.325,-0.65));
#21748=CARTESIAN_POINT('Ctrl Pts',(-0.0324967135411163,-0.328153081062251,
-0.649370620646074));
#21749=CARTESIAN_POINT('Ctrl Pts',(-0.0632828231545122,-0.340922081922822,
-0.647096224417991));
#21750=CARTESIAN_POINT('Ctrl Pts',(-0.0773125544088348,-0.350535859112198,
-0.645482573914132));
#21751=CARTESIAN_POINT('Ctrl Pts',(-0.0994646698947639,-0.372687974598127,
-0.642442040715078));
#21752=CARTESIAN_POINT('Ctrl Pts',(-0.109078032552995,-0.386717480603274,
-0.640815160902589));
#21753=CARTESIAN_POINT('Ctrl Pts',(-0.121846732641678,-0.417502809542363,
-0.63851034608138));
#21754=CARTESIAN_POINT('Ctrl Pts',(-0.125,-0.434262111007648,-0.637867541108654));
#21755=CARTESIAN_POINT('Ctrl Pts',(-0.125,-0.45,-0.637867541108654));
#21756=CARTESIAN_POINT('Ctrl Pts',(-0.125,-0.45,-0.637867541108654));
#21757=CARTESIAN_POINT('Ctrl Pts',(-0.125,-0.465737888992352,-0.637867541108654));
#21758=CARTESIAN_POINT('Ctrl Pts',(-0.121846732641678,-0.482497190457636,
-0.63851034608138));
#21759=CARTESIAN_POINT('Ctrl Pts',(-0.109078032552995,-0.513282519396725,
-0.640815160902589));
#21760=CARTESIAN_POINT('Ctrl Pts',(-0.099464669894764,-0.527312025401873,
-0.642442040715078));
#21761=CARTESIAN_POINT('Ctrl Pts',(-0.0773125544088349,-0.549464140887802,
-0.645482573914132));
#21762=CARTESIAN_POINT('Ctrl Pts',(-0.0632828231545124,-0.559077918077178,
-0.647096224417991));
#21763=CARTESIAN_POINT('Ctrl Pts',(-0.0324967135411165,-0.571846918937749,
-0.649370620646074));
#21764=CARTESIAN_POINT('Ctrl Pts',(-0.0157371373481998,-0.575,-0.65));
#21765=CARTESIAN_POINT('Ctrl Pts',(-1.73472347597681E-17,-0.575,-0.65));
#21766=CARTESIAN_POINT('',(0.,-0.325,0.65));
#21767=CARTESIAN_POINT('',(0.,-0.575,0.65));
#21768=CARTESIAN_POINT('Ctrl Pts',(2.77555756156289E-17,-0.325,0.65));
#21769=CARTESIAN_POINT('Ctrl Pts',(0.0157371373481998,-0.325,0.65));
#21770=CARTESIAN_POINT('Ctrl Pts',(0.0324967135411164,-0.328153081062251,
0.649370620646074));
#21771=CARTESIAN_POINT('Ctrl Pts',(0.0632828231545123,-0.340922081922822,
0.647096224417991));
#21772=CARTESIAN_POINT('Ctrl Pts',(0.0773125544088349,-0.350535859112198,
0.645482573914132));
#21773=CARTESIAN_POINT('Ctrl Pts',(0.099464669894764,-0.372687974598127,
0.642442040715078));
#21774=CARTESIAN_POINT('Ctrl Pts',(0.109078032552995,-0.386717480603275,
0.640815160902589));
#21775=CARTESIAN_POINT('Ctrl Pts',(0.121846732641678,-0.417502809542364,
0.63851034608138));
#21776=CARTESIAN_POINT('Ctrl Pts',(0.125,-0.434262111007648,0.637867541108654));
#21777=CARTESIAN_POINT('Ctrl Pts',(0.125,-0.465737888992352,0.637867541108654));
#21778=CARTESIAN_POINT('Ctrl Pts',(0.121846732641678,-0.482497190457636,
0.63851034608138));
#21779=CARTESIAN_POINT('Ctrl Pts',(0.109078032552995,-0.513282519396725,
0.640815160902589));
#21780=CARTESIAN_POINT('Ctrl Pts',(0.099464669894764,-0.527312025401873,
0.642442040715078));
#21781=CARTESIAN_POINT('Ctrl Pts',(0.077312554408835,-0.549464140887802,
0.645482573914132));
#21782=CARTESIAN_POINT('Ctrl Pts',(0.0632828231545124,-0.559077918077178,
0.647096224417991));
#21783=CARTESIAN_POINT('Ctrl Pts',(0.0324967135411165,-0.571846918937749,
0.649370620646074));
#21784=CARTESIAN_POINT('Ctrl Pts',(0.0157371373481998,-0.575,0.65));
#21785=CARTESIAN_POINT('Ctrl Pts',(-1.38777878078145E-17,-0.575,0.65));
#21786=CARTESIAN_POINT('',(-0.125,-0.45,0.637867541108654));
#21787=CARTESIAN_POINT('Ctrl Pts',(-1.04083408558608E-17,-0.575,0.65));
#21788=CARTESIAN_POINT('Ctrl Pts',(-0.0157371373481998,-0.575,0.65));
#21789=CARTESIAN_POINT('Ctrl Pts',(-0.0324967135411164,-0.571846918937749,
0.649370620646074));
#21790=CARTESIAN_POINT('Ctrl Pts',(-0.0632828231545123,-0.559077918077178,
0.647096224417991));
#21791=CARTESIAN_POINT('Ctrl Pts',(-0.0773125544088349,-0.549464140887802,
0.645482573914132));
#21792=CARTESIAN_POINT('Ctrl Pts',(-0.099464669894764,-0.527312025401873,
0.642442040715078));
#21793=CARTESIAN_POINT('Ctrl Pts',(-0.109078032552995,-0.513282519396725,
0.640815160902589));
#21794=CARTESIAN_POINT('Ctrl Pts',(-0.121846732641678,-0.482497190457636,
0.63851034608138));
#21795=CARTESIAN_POINT('Ctrl Pts',(-0.125,-0.465737888992352,0.637867541108654));
#21796=CARTESIAN_POINT('Ctrl Pts',(-0.125,-0.45,0.637867541108654));
#21797=CARTESIAN_POINT('Ctrl Pts',(-0.125,-0.45,0.637867541108654));
#21798=CARTESIAN_POINT('Ctrl Pts',(-0.125,-0.434262111007648,0.637867541108654));
#21799=CARTESIAN_POINT('Ctrl Pts',(-0.121846732641678,-0.417502809542363,
0.63851034608138));
#21800=CARTESIAN_POINT('Ctrl Pts',(-0.109078032552995,-0.386717480603274,
0.640815160902589));
#21801=CARTESIAN_POINT('Ctrl Pts',(-0.0994646698947639,-0.372687974598127,
0.642442040715078));
#21802=CARTESIAN_POINT('Ctrl Pts',(-0.0773125544088348,-0.350535859112198,
0.645482573914132));
#21803=CARTESIAN_POINT('Ctrl Pts',(-0.0632828231545122,-0.340922081922822,
0.647096224417991));
#21804=CARTESIAN_POINT('Ctrl Pts',(-0.0324967135411163,-0.328153081062251,
0.649370620646074));
#21805=CARTESIAN_POINT('Ctrl Pts',(-0.0157371373481998,-0.325,0.65));
#21806=CARTESIAN_POINT('Ctrl Pts',(4.5102810375397E-17,-0.325,0.65));
#21807=CARTESIAN_POINT('Origin',(0.,-0.45,0.));
#21808=CARTESIAN_POINT('',(-0.125,-0.45,-0.379967103839267));
#21809=CARTESIAN_POINT('',(-0.125,-0.45,0.));
#21810=CARTESIAN_POINT('',(0.125,-0.45,-0.379967103839267));
#21811=CARTESIAN_POINT('Ctrl Pts',(0.125,-0.45,-0.379967103839267));
#21812=CARTESIAN_POINT('Ctrl Pts',(0.125,-0.465813100629203,-0.379967103839267));
#21813=CARTESIAN_POINT('Ctrl Pts',(0.121817958968287,-0.48260129709332,
-0.381057715344782));
#21814=CARTESIAN_POINT('Ctrl Pts',(0.109029967924066,-0.51336346023721,
-0.384911758361269));
#21815=CARTESIAN_POINT('Ctrl Pts',(0.0994291026068839,-0.527347592689753,
-0.38761064154154));
#21816=CARTESIAN_POINT('Ctrl Pts',(0.0773514949786257,-0.549425200318011,
-0.392612801026882));
#21817=CARTESIAN_POINT('Ctrl Pts',(0.0633657881355918,-0.559029081159106,
-0.395252954914593));
#21818=CARTESIAN_POINT('Ctrl Pts',(0.0325978607437828,-0.571819306519379,
-0.398970551469948));
#21819=CARTESIAN_POINT('Ctrl Pts',(0.0158075115832676,-0.575,-0.4));
#21820=CARTESIAN_POINT('Ctrl Pts',(-0.0158075115832676,-0.575,-0.4));
#21821=CARTESIAN_POINT('Ctrl Pts',(-0.0325978607437828,-0.571819306519379,
-0.398970551469948));
#21822=CARTESIAN_POINT('Ctrl Pts',(-0.0633657881355918,-0.559029081159106,
-0.395252954914593));
#21823=CARTESIAN_POINT('Ctrl Pts',(-0.0773514949786256,-0.549425200318011,
-0.392612801026882));
#21824=CARTESIAN_POINT('Ctrl Pts',(-0.0994291026068839,-0.527347592689753,
-0.38761064154154));
#21825=CARTESIAN_POINT('Ctrl Pts',(-0.109029967924066,-0.51336346023721,
-0.384911758361269));
#21826=CARTESIAN_POINT('Ctrl Pts',(-0.121817958968287,-0.48260129709332,
-0.381057715344782));
#21827=CARTESIAN_POINT('Ctrl Pts',(-0.125,-0.465813100629203,-0.379967103839267));
#21828=CARTESIAN_POINT('Ctrl Pts',(-0.125,-0.45,-0.379967103839267));
#21829=CARTESIAN_POINT('Ctrl Pts',(-0.125,-0.45,-0.379967103839267));
#21830=CARTESIAN_POINT('Ctrl Pts',(-0.125,-0.434186899370797,-0.379967103839267));
#21831=CARTESIAN_POINT('Ctrl Pts',(-0.121817958968287,-0.41739870290668,
-0.381057715344782));
#21832=CARTESIAN_POINT('Ctrl Pts',(-0.109029967924066,-0.38663653976279,
-0.384911758361269));
#21833=CARTESIAN_POINT('Ctrl Pts',(-0.0994291026068839,-0.372652407310247,
-0.38761064154154));
#21834=CARTESIAN_POINT('Ctrl Pts',(-0.0773514949786257,-0.350574799681989,
-0.392612801026882));
#21835=CARTESIAN_POINT('Ctrl Pts',(-0.0633657881355918,-0.340970918840894,
-0.395252954914593));
#21836=CARTESIAN_POINT('Ctrl Pts',(-0.0325978607437829,-0.328180693480621,
-0.398970551469948));
#21837=CARTESIAN_POINT('Ctrl Pts',(-0.0158075115832676,-0.325,-0.4));
#21838=CARTESIAN_POINT('Ctrl Pts',(0.0158075115832675,-0.325,-0.4));
#21839=CARTESIAN_POINT('Ctrl Pts',(0.0325978607437828,-0.328180693480621,
-0.398970551469948));
#21840=CARTESIAN_POINT('Ctrl Pts',(0.0633657881355917,-0.340970918840894,
-0.395252954914593));
#21841=CARTESIAN_POINT('Ctrl Pts',(0.0773514949786256,-0.350574799681989,
-0.392612801026882));
#21842=CARTESIAN_POINT('Ctrl Pts',(0.0994291026068839,-0.372652407310247,
-0.38761064154154));
#21843=CARTESIAN_POINT('Ctrl Pts',(0.109029967924066,-0.38663653976279,
-0.384911758361269));
#21844=CARTESIAN_POINT('Ctrl Pts',(0.121817958968287,-0.41739870290668,
-0.381057715344782));
#21845=CARTESIAN_POINT('Ctrl Pts',(0.125,-0.434186899370797,-0.379967103839267));
#21846=CARTESIAN_POINT('Ctrl Pts',(0.125,-0.45,-0.379967103839267));
#21847=CARTESIAN_POINT('Origin',(0.,-0.45,0.));
#21848=CARTESIAN_POINT('',(0.125,-0.45,0.379967103839267));
#21849=CARTESIAN_POINT('',(-0.125,-0.45,0.379967103839267));
#21850=CARTESIAN_POINT('Ctrl Pts',(0.125,-0.45,0.379967103839267));
#21851=CARTESIAN_POINT('Ctrl Pts',(0.125,-0.434186899370797,0.379967103839267));
#21852=CARTESIAN_POINT('Ctrl Pts',(0.121817958968287,-0.41739870290668,
0.381057715344782));
#21853=CARTESIAN_POINT('Ctrl Pts',(0.109029967924066,-0.38663653976279,
0.384911758361269));
#21854=CARTESIAN_POINT('Ctrl Pts',(0.0994291026068839,-0.372652407310247,
0.38761064154154));
#21855=CARTESIAN_POINT('Ctrl Pts',(0.0773514949786256,-0.350574799681989,
0.392612801026882));
#21856=CARTESIAN_POINT('Ctrl Pts',(0.0633657881355918,-0.340970918840894,
0.395252954914593));
#21857=CARTESIAN_POINT('Ctrl Pts',(0.0325978607437828,-0.328180693480621,
0.398970551469948));
#21858=CARTESIAN_POINT('Ctrl Pts',(0.0158075115832676,-0.325,0.4));
#21859=CARTESIAN_POINT('Ctrl Pts',(-0.0158075115832676,-0.325,0.4));
#21860=CARTESIAN_POINT('Ctrl Pts',(-0.0325978607437828,-0.328180693480621,
0.398970551469948));
#21861=CARTESIAN_POINT('Ctrl Pts',(-0.0633657881355918,-0.340970918840894,
0.395252954914593));
#21862=CARTESIAN_POINT('Ctrl Pts',(-0.0773514949786257,-0.350574799681989,
0.392612801026882));
#21863=CARTESIAN_POINT('Ctrl Pts',(-0.0994291026068839,-0.372652407310247,
0.38761064154154));
#21864=CARTESIAN_POINT('Ctrl Pts',(-0.109029967924066,-0.38663653976279,
0.384911758361269));
#21865=CARTESIAN_POINT('Ctrl Pts',(-0.121817958968287,-0.41739870290668,
0.381057715344782));
#21866=CARTESIAN_POINT('Ctrl Pts',(-0.125,-0.434186899370797,0.379967103839267));
#21867=CARTESIAN_POINT('Ctrl Pts',(-0.125,-0.45,0.379967103839267));
#21868=CARTESIAN_POINT('Ctrl Pts',(-0.125,-0.45,0.379967103839267));
#21869=CARTESIAN_POINT('Ctrl Pts',(-0.125,-0.465813100629203,0.379967103839267));
#21870=CARTESIAN_POINT('Ctrl Pts',(-0.121817958968287,-0.48260129709332,
0.381057715344782));
#21871=CARTESIAN_POINT('Ctrl Pts',(-0.109029967924066,-0.51336346023721,
0.384911758361269));
#21872=CARTESIAN_POINT('Ctrl Pts',(-0.0994291026068839,-0.527347592689753,
0.38761064154154));
#21873=CARTESIAN_POINT('Ctrl Pts',(-0.0773514949786256,-0.549425200318011,
0.392612801026882));
#21874=CARTESIAN_POINT('Ctrl Pts',(-0.0633657881355917,-0.559029081159106,
0.395252954914593));
#21875=CARTESIAN_POINT('Ctrl Pts',(-0.0325978607437828,-0.571819306519379,
0.398970551469948));
#21876=CARTESIAN_POINT('Ctrl Pts',(-0.0158075115832675,-0.575,0.4));
#21877=CARTESIAN_POINT('Ctrl Pts',(0.0158075115832676,-0.575,0.4));
#21878=CARTESIAN_POINT('Ctrl Pts',(0.0325978607437828,-0.571819306519379,
0.398970551469948));
#21879=CARTESIAN_POINT('Ctrl Pts',(0.0633657881355917,-0.559029081159106,
0.395252954914593));
#21880=CARTESIAN_POINT('Ctrl Pts',(0.0773514949786257,-0.549425200318011,
0.392612801026882));
#21881=CARTESIAN_POINT('Ctrl Pts',(0.0994291026068839,-0.527347592689753,
0.38761064154154));
#21882=CARTESIAN_POINT('Ctrl Pts',(0.109029967924066,-0.51336346023721,
0.384911758361269));
#21883=CARTESIAN_POINT('Ctrl Pts',(0.121817958968287,-0.48260129709332,
0.381057715344782));
#21884=CARTESIAN_POINT('Ctrl Pts',(0.125,-0.465813100629203,0.379967103839267));
#21885=CARTESIAN_POINT('Ctrl Pts',(0.125,-0.45,0.379967103839267));
#21886=CARTESIAN_POINT('',(-0.125,-0.45,0.));
#21887=CARTESIAN_POINT('Origin',(0.,0.,0.));
#21888=CARTESIAN_POINT('',(-0.4,-0.8,4.89858719658941E-17));
#21889=CARTESIAN_POINT('Origin',(0.,-0.8,0.));
#21890=CARTESIAN_POINT('',(-0.4,0.,4.89858719658941E-17));
#21891=CARTESIAN_POINT('',(-0.4,0.85,-4.89858719658941E-17));
#21892=CARTESIAN_POINT('',(-0.4,0.,4.89858719658941E-17));
#21893=CARTESIAN_POINT('Origin',(0.,0.85,0.));
#21894=CARTESIAN_POINT('Origin',(0.,-0.8,0.));
#21895=CARTESIAN_POINT('Origin',(0.,0.,0.));
#21896=CARTESIAN_POINT('',(-0.8,0.,9.79717439317883E-17));
#21897=CARTESIAN_POINT('Origin',(0.,0.,0.));
#21898=CARTESIAN_POINT('',(0.595438916863769,0.,0.137993139022126));
#21899=CARTESIAN_POINT('',(0.562830534889751,0.,0.238351419397483));
#21900=CARTESIAN_POINT('Origin',(0.562758945330873,0.,0.182851465569258));
#21901=CARTESIAN_POINT('',(0.523653836874034,0.,0.315240018494132));
#21902=CARTESIAN_POINT('Origin',(0.,0.,0.));
#21903=CARTESIAN_POINT('',(0.461629008549572,0.,0.40060987082025));
#21904=CARTESIAN_POINT('Origin',(0.478711351753049,0.,0.347804155687524));
#21905=CARTESIAN_POINT('',(0.40060987082025,0.,0.461629008549572));
#21906=CARTESIAN_POINT('Origin',(0.,0.,0.));
#21907=CARTESIAN_POINT('',(0.315240018494132,0.,0.523653836874034));
#21908=CARTESIAN_POINT('Origin',(0.347804155687523,0.,0.478711351753049));
#21909=CARTESIAN_POINT('',(0.238351419397483,0.,0.562830534889751));
#21910=CARTESIAN_POINT('Origin',(0.,0.,0.));
#21911=CARTESIAN_POINT('',(0.137993139022126,0.,0.595438916863769));
#21912=CARTESIAN_POINT('Origin',(0.182851465569258,0.,0.562758945330873));
#21913=CARTESIAN_POINT('',(0.0527614703521001,0.,0.608938287003997));
#21914=CARTESIAN_POINT('Origin',(0.,0.,0.));
#21915=CARTESIAN_POINT('',(-0.0527614703521003,0.,0.608938287003997));
#21916=CARTESIAN_POINT('Origin',(-1.08697158783324E-16,0.,0.591719772367581));
#21917=CARTESIAN_POINT('',(-0.137993139022126,0.,0.595438916863769));
#21918=CARTESIAN_POINT('Origin',(0.,0.,0.));
#21919=CARTESIAN_POINT('',(-0.238351419397483,0.,0.562830534889751));
#21920=CARTESIAN_POINT('Origin',(-0.182851465569258,0.,0.562758945330873));
#21921=CARTESIAN_POINT('',(-0.315240018494132,0.,0.523653836874034));
#21922=CARTESIAN_POINT('Origin',(0.,0.,0.));
#21923=CARTESIAN_POINT('',(-0.40060987082025,0.,0.461629008549572));
#21924=CARTESIAN_POINT('Origin',(-0.347804155687524,0.,0.478711351753049));
#21925=CARTESIAN_POINT('',(-0.461629008549572,0.,0.40060987082025));
#21926=CARTESIAN_POINT('Origin',(0.,0.,0.));
#21927=CARTESIAN_POINT('',(-0.523653836874034,0.,0.315240018494132));
#21928=CARTESIAN_POINT('Origin',(-0.478711351753049,0.,0.347804155687524));
#21929=CARTESIAN_POINT('',(-0.562830534889751,0.,0.238351419397483));
#21930=CARTESIAN_POINT('Origin',(0.,0.,0.));
#21931=CARTESIAN_POINT('',(-0.595438916863769,0.,0.137993139022126));
#21932=CARTESIAN_POINT('Origin',(-0.562758945330873,0.,0.182851465569258));
#21933=CARTESIAN_POINT('',(-0.608938287003997,0.,0.0527614703521002));
#21934=CARTESIAN_POINT('Origin',(0.,0.,0.));
#21935=CARTESIAN_POINT('',(-0.608938287003997,0.,-0.0527614703521003));
#21936=CARTESIAN_POINT('Origin',(-0.591719772367581,0.,-7.24647725222159E-17));
#21937=CARTESIAN_POINT('',(-0.595438916863769,0.,-0.137993139022126));
#21938=CARTESIAN_POINT('Origin',(0.,0.,0.));
#21939=CARTESIAN_POINT('',(-0.562830534889751,0.,-0.238351419397483));
#21940=CARTESIAN_POINT('Origin',(-0.562758945330873,0.,-0.182851465569258));
#21941=CARTESIAN_POINT('',(-0.523653836874034,0.,-0.315240018494132));
#21942=CARTESIAN_POINT('Origin',(0.,0.,0.));
#21943=CARTESIAN_POINT('',(-0.461629008549572,0.,-0.40060987082025));
#21944=CARTESIAN_POINT('Origin',(-0.478711351753049,0.,-0.347804155687524));
#21945=CARTESIAN_POINT('',(-0.40060987082025,0.,-0.461629008549572));
#21946=CARTESIAN_POINT('Origin',(0.,0.,0.));
#21947=CARTESIAN_POINT('',(-0.315240018494132,0.,-0.523653836874034));
#21948=CARTESIAN_POINT('Origin',(-0.347804155687524,0.,-0.478711351753049));
#21949=CARTESIAN_POINT('',(-0.238351419397483,0.,-0.562830534889751));
#21950=CARTESIAN_POINT('Origin',(0.,0.,0.));
#21951=CARTESIAN_POINT('',(-0.137993139022126,0.,-0.595438916863769));
#21952=CARTESIAN_POINT('Origin',(-0.182851465569258,0.,-0.562758945330873));
#21953=CARTESIAN_POINT('',(-0.0527614703521002,0.,-0.608938287003997));
#21954=CARTESIAN_POINT('Origin',(0.,0.,0.));
#21955=CARTESIAN_POINT('',(0.0527614703521003,0.,-0.608938287003997));
#21956=CARTESIAN_POINT('Origin',(3.6232386261108E-17,0.,-0.591719772367581));
#21957=CARTESIAN_POINT('',(0.137993139022126,0.,-0.595438916863769));
#21958=CARTESIAN_POINT('Origin',(0.,0.,0.));
#21959=CARTESIAN_POINT('',(0.238351419397483,0.,-0.562830534889751));
#21960=CARTESIAN_POINT('Origin',(0.182851465569258,0.,-0.562758945330873));
#21961=CARTESIAN_POINT('',(0.315240018494132,0.,-0.523653836874034));
#21962=CARTESIAN_POINT('Origin',(0.,0.,0.));
#21963=CARTESIAN_POINT('',(0.40060987082025,0.,-0.461629008549572));
#21964=CARTESIAN_POINT('Origin',(0.347804155687524,0.,-0.478711351753049));
#21965=CARTESIAN_POINT('',(0.461629008549572,0.,-0.40060987082025));
#21966=CARTESIAN_POINT('Origin',(0.,0.,0.));
#21967=CARTESIAN_POINT('',(0.523653836874034,0.,-0.315240018494132));
#21968=CARTESIAN_POINT('Origin',(0.478711351753049,0.,-0.347804155687524));
#21969=CARTESIAN_POINT('',(0.562830534889751,0.,-0.238351419397483));
#21970=CARTESIAN_POINT('Origin',(0.,0.,0.));
#21971=CARTESIAN_POINT('',(0.595438916863769,0.,-0.137993139022126));
#21972=CARTESIAN_POINT('Origin',(0.562758945330873,0.,-0.182851465569258));
#21973=CARTESIAN_POINT('',(0.608938287003997,0.,-0.0527614703521001));
#21974=CARTESIAN_POINT('Origin',(0.,0.,0.));
#21975=CARTESIAN_POINT('',(0.608938287003997,0.,0.0527614703521001));
#21976=CARTESIAN_POINT('Origin',(0.591719772367581,0.,0.));
#21977=CARTESIAN_POINT('Origin',(0.,0.,0.));
#21978=CARTESIAN_POINT('Origin',(0.,0.,0.));
#21979=CARTESIAN_POINT('',(-0.8,-0.1,9.79717439317883E-17));
#21980=CARTESIAN_POINT('Origin',(0.,-0.1,0.));
#21981=CARTESIAN_POINT('',(-0.8,0.,-9.79717439317883E-17));
#21982=CARTESIAN_POINT('Origin',(0.,-0.1,0.));
#21983=CARTESIAN_POINT('Origin',(0.,0.75,0.));
#21984=CARTESIAN_POINT('',(-0.8,0.75,9.79717439317883E-17));
#21985=CARTESIAN_POINT('Origin',(0.,0.75,0.));
#21986=CARTESIAN_POINT('',(0.562830534889751,0.75,0.238351419397483));
#21987=CARTESIAN_POINT('',(0.595438916863769,0.75,0.137993139022126));
#21988=CARTESIAN_POINT('Origin',(0.562758945330873,0.75,0.182851465569258));
#21989=CARTESIAN_POINT('',(0.608938287003997,0.75,0.0527614703521002));
#21990=CARTESIAN_POINT('Origin',(0.,0.75,0.));
#21991=CARTESIAN_POINT('',(0.608938287003997,0.75,-0.0527614703521002));
#21992=CARTESIAN_POINT('Origin',(0.591719772367581,0.75,0.));
#21993=CARTESIAN_POINT('',(0.595438916863769,0.75,-0.137993139022126));
#21994=CARTESIAN_POINT('Origin',(0.,0.75,0.));
#21995=CARTESIAN_POINT('',(0.562830534889751,0.75,-0.238351419397483));
#21996=CARTESIAN_POINT('Origin',(0.562758945330873,0.75,-0.182851465569258));
#21997=CARTESIAN_POINT('',(0.523653836874034,0.75,-0.315240018494132));
#21998=CARTESIAN_POINT('Origin',(0.,0.75,0.));
#21999=CARTESIAN_POINT('',(0.461629008549572,0.75,-0.40060987082025));
#22000=CARTESIAN_POINT('Origin',(0.478711351753049,0.75,-0.347804155687524));
#22001=CARTESIAN_POINT('',(0.40060987082025,0.75,-0.461629008549572));
#22002=CARTESIAN_POINT('Origin',(0.,0.75,0.));
#22003=CARTESIAN_POINT('',(0.315240018494132,0.75,-0.523653836874034));
#22004=CARTESIAN_POINT('Origin',(0.347804155687524,0.75,-0.478711351753049));
#22005=CARTESIAN_POINT('',(0.238351419397483,0.75,-0.562830534889751));
#22006=CARTESIAN_POINT('Origin',(0.,0.75,0.));
#22007=CARTESIAN_POINT('',(0.137993139022126,0.75,-0.595438916863769));
#22008=CARTESIAN_POINT('Origin',(0.182851465569258,0.75,-0.562758945330873));
#22009=CARTESIAN_POINT('',(0.0527614703521003,0.75,-0.608938287003997));
#22010=CARTESIAN_POINT('Origin',(0.,0.75,0.));
#22011=CARTESIAN_POINT('',(-0.0527614703521002,0.75,-0.608938287003997));
#22012=CARTESIAN_POINT('Origin',(3.6232386261108E-17,0.75,-0.591719772367581));
#22013=CARTESIAN_POINT('',(-0.137993139022126,0.75,-0.595438916863769));
#22014=CARTESIAN_POINT('Origin',(0.,0.75,0.));
#22015=CARTESIAN_POINT('',(-0.238351419397483,0.75,-0.562830534889751));
#22016=CARTESIAN_POINT('Origin',(-0.182851465569258,0.75,-0.562758945330873));
#22017=CARTESIAN_POINT('',(-0.315240018494132,0.75,-0.523653836874034));
#22018=CARTESIAN_POINT('Origin',(0.,0.75,0.));
#22019=CARTESIAN_POINT('',(-0.40060987082025,0.75,-0.461629008549572));
#22020=CARTESIAN_POINT('Origin',(-0.347804155687524,0.75,-0.478711351753049));
#22021=CARTESIAN_POINT('',(-0.461629008549572,0.75,-0.40060987082025));
#22022=CARTESIAN_POINT('Origin',(0.,0.75,0.));
#22023=CARTESIAN_POINT('',(-0.523653836874034,0.75,-0.315240018494132));
#22024=CARTESIAN_POINT('Origin',(-0.478711351753049,0.75,-0.347804155687524));
#22025=CARTESIAN_POINT('',(-0.562830534889751,0.75,-0.238351419397483));
#22026=CARTESIAN_POINT('Origin',(0.,0.75,0.));
#22027=CARTESIAN_POINT('',(-0.595438916863769,0.75,-0.137993139022126));
#22028=CARTESIAN_POINT('Origin',(-0.562758945330873,0.75,-0.182851465569258));
#22029=CARTESIAN_POINT('',(-0.608938287003997,0.75,-0.0527614703521003));
#22030=CARTESIAN_POINT('Origin',(0.,0.75,0.));
#22031=CARTESIAN_POINT('',(-0.608938287003997,0.75,0.0527614703521002));
#22032=CARTESIAN_POINT('Origin',(-0.591719772367581,0.75,-7.24647725222159E-17));
#22033=CARTESIAN_POINT('',(-0.595438916863769,0.75,0.137993139022126));
#22034=CARTESIAN_POINT('Origin',(0.,0.75,0.));
#22035=CARTESIAN_POINT('',(-0.562830534889751,0.75,0.238351419397483));
#22036=CARTESIAN_POINT('Origin',(-0.562758945330873,0.75,0.182851465569258));
#22037=CARTESIAN_POINT('',(-0.523653836874034,0.75,0.315240018494132));
#22038=CARTESIAN_POINT('Origin',(0.,0.75,0.));
#22039=CARTESIAN_POINT('',(-0.461629008549572,0.75,0.40060987082025));
#22040=CARTESIAN_POINT('Origin',(-0.478711351753049,0.75,0.347804155687524));
#22041=CARTESIAN_POINT('',(-0.40060987082025,0.75,0.461629008549572));
#22042=CARTESIAN_POINT('Origin',(0.,0.75,0.));
#22043=CARTESIAN_POINT('',(-0.315240018494132,0.75,0.523653836874034));
#22044=CARTESIAN_POINT('Origin',(-0.347804155687524,0.75,0.478711351753049));
#22045=CARTESIAN_POINT('',(-0.238351419397483,0.75,0.562830534889751));
#22046=CARTESIAN_POINT('Origin',(0.,0.75,0.));
#22047=CARTESIAN_POINT('',(-0.137993139022126,0.75,0.595438916863769));
#22048=CARTESIAN_POINT('Origin',(-0.182851465569258,0.75,0.562758945330873));
#22049=CARTESIAN_POINT('',(-0.0527614703521003,0.75,0.608938287003997));
#22050=CARTESIAN_POINT('Origin',(0.,0.75,0.));
#22051=CARTESIAN_POINT('',(0.0527614703521001,0.75,0.608938287003997));
#22052=CARTESIAN_POINT('Origin',(-1.08697158783324E-16,0.75,0.591719772367581));
#22053=CARTESIAN_POINT('',(0.137993139022126,0.75,0.595438916863769));
#22054=CARTESIAN_POINT('Origin',(0.,0.75,0.));
#22055=CARTESIAN_POINT('',(0.238351419397483,0.75,0.562830534889751));
#22056=CARTESIAN_POINT('Origin',(0.182851465569258,0.75,0.562758945330873));
#22057=CARTESIAN_POINT('',(0.315240018494132,0.75,0.523653836874034));
#22058=CARTESIAN_POINT('Origin',(0.,0.75,0.));
#22059=CARTESIAN_POINT('',(0.40060987082025,0.75,0.461629008549572));
#22060=CARTESIAN_POINT('Origin',(0.347804155687523,0.75,0.478711351753049));
#22061=CARTESIAN_POINT('',(0.461629008549572,0.75,0.40060987082025));
#22062=CARTESIAN_POINT('Origin',(0.,0.75,0.));
#22063=CARTESIAN_POINT('',(0.523653836874034,0.75,0.315240018494132));
#22064=CARTESIAN_POINT('Origin',(0.478711351753049,0.75,0.347804155687524));
#22065=CARTESIAN_POINT('Origin',(0.,0.75,0.));
#22066=CARTESIAN_POINT('Origin',(0.,0.75,0.));
#22067=CARTESIAN_POINT('',(-0.8,0.85,9.79717439317883E-17));
#22068=CARTESIAN_POINT('Origin',(0.,0.85,0.));
#22069=CARTESIAN_POINT('',(-0.8,0.75,9.79717439317883E-17));
#22070=CARTESIAN_POINT('Origin',(0.,0.85,0.));
#22071=CARTESIAN_POINT('Origin',(0.562758945330873,0.,0.182851465569258));
#22072=CARTESIAN_POINT('',(0.595438916863769,0.,0.137993139022126));
#22073=CARTESIAN_POINT('',(0.562830534889751,0.,0.238351419397483));
#22074=CARTESIAN_POINT('Origin',(0.,0.,0.));
#22075=CARTESIAN_POINT('',(0.523653836874034,0.,0.315240018494132));
#22076=CARTESIAN_POINT('Origin',(0.478711351753049,0.,0.347804155687524));
#22077=CARTESIAN_POINT('',(0.461629008549572,0.,0.40060987082025));
#22078=CARTESIAN_POINT('Origin',(0.,0.,0.));
#22079=CARTESIAN_POINT('',(0.40060987082025,0.,0.461629008549572));
#22080=CARTESIAN_POINT('Origin',(0.347804155687523,0.,0.478711351753049));
#22081=CARTESIAN_POINT('',(0.315240018494132,0.,0.523653836874034));
#22082=CARTESIAN_POINT('Origin',(0.,0.,0.));
#22083=CARTESIAN_POINT('',(0.238351419397483,0.,0.562830534889751));
#22084=CARTESIAN_POINT('Origin',(0.182851465569258,0.,0.562758945330873));
#22085=CARTESIAN_POINT('',(0.137993139022126,0.,0.595438916863769));
#22086=CARTESIAN_POINT('Origin',(0.,0.,0.));
#22087=CARTESIAN_POINT('',(0.0527614703521,0.,0.608938287003997));
#22088=CARTESIAN_POINT('Origin',(-1.08697158783324E-16,0.,0.591719772367581));
#22089=CARTESIAN_POINT('',(-0.0527614703521002,0.,0.608938287003997));
#22090=CARTESIAN_POINT('Origin',(0.,0.,0.));
#22091=CARTESIAN_POINT('',(-0.137993139022126,0.,0.595438916863769));
#22092=CARTESIAN_POINT('Origin',(-0.182851465569258,0.,0.562758945330873));
#22093=CARTESIAN_POINT('',(-0.238351419397483,0.,0.562830534889751));
#22094=CARTESIAN_POINT('Origin',(0.,0.,0.));
#22095=CARTESIAN_POINT('',(-0.315240018494132,0.,0.523653836874034));
#22096=CARTESIAN_POINT('Origin',(-0.347804155687524,0.,0.478711351753049));
#22097=CARTESIAN_POINT('',(-0.40060987082025,0.,0.461629008549572));
#22098=CARTESIAN_POINT('Origin',(0.,0.,0.));
#22099=CARTESIAN_POINT('',(-0.461629008549572,0.,0.40060987082025));
#22100=CARTESIAN_POINT('Origin',(-0.478711351753049,0.,0.347804155687524));
#22101=CARTESIAN_POINT('',(-0.523653836874034,0.,0.315240018494132));
#22102=CARTESIAN_POINT('Origin',(0.,0.,0.));
#22103=CARTESIAN_POINT('',(-0.562830534889751,0.,0.238351419397483));
#22104=CARTESIAN_POINT('Origin',(-0.562758945330873,0.,0.182851465569258));
#22105=CARTESIAN_POINT('',(-0.595438916863769,0.,0.137993139022126));
#22106=CARTESIAN_POINT('Origin',(0.,0.,0.));
#22107=CARTESIAN_POINT('',(-0.608938287003997,0.,0.0527614703521));
#22108=CARTESIAN_POINT('Origin',(-0.591719772367581,0.,-7.24647725222159E-17));
#22109=CARTESIAN_POINT('',(-0.608938287003997,0.,-0.0527614703521002));
#22110=CARTESIAN_POINT('Origin',(0.,0.,0.));
#22111=CARTESIAN_POINT('',(-0.595438916863769,0.,-0.137993139022126));
#22112=CARTESIAN_POINT('Origin',(-0.562758945330873,0.,-0.182851465569258));
#22113=CARTESIAN_POINT('',(-0.562830534889751,0.,-0.238351419397483));
#22114=CARTESIAN_POINT('Origin',(0.,0.,0.));
#22115=CARTESIAN_POINT('',(-0.523653836874034,0.,-0.315240018494132));
#22116=CARTESIAN_POINT('Origin',(-0.478711351753049,0.,-0.347804155687524));
#22117=CARTESIAN_POINT('',(-0.461629008549572,0.,-0.40060987082025));
#22118=CARTESIAN_POINT('Origin',(0.,0.,0.));
#22119=CARTESIAN_POINT('',(-0.40060987082025,0.,-0.461629008549572));
#22120=CARTESIAN_POINT('Origin',(-0.347804155687524,0.,-0.478711351753049));
#22121=CARTESIAN_POINT('',(-0.315240018494132,0.,-0.523653836874034));
#22122=CARTESIAN_POINT('Origin',(0.,0.,0.));
#22123=CARTESIAN_POINT('',(-0.238351419397483,0.,-0.562830534889751));
#22124=CARTESIAN_POINT('Origin',(-0.182851465569258,0.,-0.562758945330873));
#22125=CARTESIAN_POINT('',(-0.137993139022126,0.,-0.595438916863769));
#22126=CARTESIAN_POINT('Origin',(0.,0.,0.));
#22127=CARTESIAN_POINT('',(-0.0527614703521,0.,-0.608938287003997));
#22128=CARTESIAN_POINT('Origin',(3.6232386261108E-17,0.,-0.591719772367581));
#22129=CARTESIAN_POINT('',(0.0527614703521001,0.,-0.608938287003997));
#22130=CARTESIAN_POINT('Origin',(0.,0.,0.));
#22131=CARTESIAN_POINT('',(0.137993139022126,0.,-0.595438916863769));
#22132=CARTESIAN_POINT('Origin',(0.182851465569258,0.,-0.562758945330873));
#22133=CARTESIAN_POINT('',(0.238351419397483,0.,-0.562830534889751));
#22134=CARTESIAN_POINT('Origin',(0.,0.,0.));
#22135=CARTESIAN_POINT('',(0.315240018494132,0.,-0.523653836874034));
#22136=CARTESIAN_POINT('Origin',(0.347804155687524,0.,-0.478711351753049));
#22137=CARTESIAN_POINT('',(0.40060987082025,0.,-0.461629008549572));
#22138=CARTESIAN_POINT('Origin',(0.,0.,0.));
#22139=CARTESIAN_POINT('',(0.461629008549572,0.,-0.40060987082025));
#22140=CARTESIAN_POINT('Origin',(0.478711351753049,0.,-0.347804155687524));
#22141=CARTESIAN_POINT('',(0.523653836874034,0.,-0.315240018494132));
#22142=CARTESIAN_POINT('Origin',(0.,0.,0.));
#22143=CARTESIAN_POINT('',(0.562830534889751,0.,-0.238351419397483));
#22144=CARTESIAN_POINT('Origin',(0.562758945330873,0.,-0.182851465569258));
#22145=CARTESIAN_POINT('',(0.595438916863769,0.,-0.137993139022126));
#22146=CARTESIAN_POINT('Origin',(0.,0.,0.));
#22147=CARTESIAN_POINT('',(0.608938287003997,0.,0.0527614703521001));
#22148=CARTESIAN_POINT('Origin',(0.591719772367581,0.,0.));
#22149=CARTESIAN_POINT('',(0.608938287003997,0.,-0.0527614703521001));
#22150=CARTESIAN_POINT('Origin',(0.,0.,0.));
#22151=CARTESIAN_POINT('',(0.,0.,0.));
#22152=CARTESIAN_POINT('',(0.,0.,0.));
#22153=CARTESIAN_POINT('Origin',(10.,-5.1,7.));
#22154=CARTESIAN_POINT('',(9.835,-5.,7.));
#22155=CARTESIAN_POINT('Origin',(10.,-5.,7.));
#22156=CARTESIAN_POINT('',(9.835,-3.4,7.));
#22157=CARTESIAN_POINT('',(9.835,-5.1,7.));
#22158=CARTESIAN_POINT('Origin',(10.,-3.4,7.));
#22159=CARTESIAN_POINT('Origin',(10.,-3.4,7.));
#22160=CARTESIAN_POINT('Origin',(10.,2.1,7.));
#22161=CARTESIAN_POINT('',(9.2,2.1,7.));
#22162=CARTESIAN_POINT('Origin',(10.,2.1,7.));
#22163=CARTESIAN_POINT('',(9.4,2.1,7.));
#22164=CARTESIAN_POINT('Origin',(10.,2.1,7.));
#22165=CARTESIAN_POINT('Origin',(10.,1.4,7.));
#22166=CARTESIAN_POINT('',(9.2,1.4,7.));
#22167=CARTESIAN_POINT('Origin',(10.,1.4,7.));
#22168=CARTESIAN_POINT('',(9.4,1.4,7.));
#22169=CARTESIAN_POINT('Origin',(10.,1.4,7.));
#22170=CARTESIAN_POINT('Origin',(10.,1.4,7.));
#22171=CARTESIAN_POINT('',(9.2,1.4,7.));
#22172=CARTESIAN_POINT('Origin',(10.,-1.8,7.));
#22173=CARTESIAN_POINT('',(9.4,-5.,7.));
#22174=CARTESIAN_POINT('',(9.4,-1.8,7.));
#22175=CARTESIAN_POINT('Origin',(10.,-5.,7.));
#22176=CARTESIAN_POINT('Origin',(10.,-5.,7.));
#22177=CARTESIAN_POINT('Origin',(10.,-1.8,7.));
#22178=CARTESIAN_POINT('',(9.4,3.,7.));
#22179=CARTESIAN_POINT('Origin',(10.,3.,7.));
#22180=CARTESIAN_POINT('',(9.4,-1.8,7.));
#22181=CARTESIAN_POINT('Origin',(10.,3.,7.));
#22182=CARTESIAN_POINT('',(0.,0.,0.));
#22183=CARTESIAN_POINT('Origin',(10.,-2.65,7.));
#22184=CARTESIAN_POINT('',(9.395,-1.4,7.));
#22185=CARTESIAN_POINT('Origin',(10.,-1.4,7.));
#22186=CARTESIAN_POINT('',(9.395,-2.65,7.));
#22187=CARTESIAN_POINT('',(9.395,-2.65,7.));
#22188=CARTESIAN_POINT('Origin',(10.,-2.65,7.));
#22189=CARTESIAN_POINT('Origin',(10.,-2.65,7.));
#22190=CARTESIAN_POINT('',(9.2,-1.4,7.));
#22191=CARTESIAN_POINT('Origin',(10.,-1.4,7.));
#22192=CARTESIAN_POINT('',(9.2,-2.65,7.));
#22193=CARTESIAN_POINT('',(9.2,-2.65,7.));
#22194=CARTESIAN_POINT('Origin',(10.,-2.65,7.));
#22195=CARTESIAN_POINT('Origin',(10.,-1.4,7.));
#22196=CARTESIAN_POINT('Origin',(10.,-2.65,7.));
#22197=CARTESIAN_POINT('',(0.,0.,0.));
#22198=CARTESIAN_POINT('Origin',(10.,-0.4,7.));
#22199=CARTESIAN_POINT('',(9.395,0.4,7.));
#22200=CARTESIAN_POINT('Origin',(10.,0.4,7.));
#22201=CARTESIAN_POINT('',(9.395,-0.4,7.));
#22202=CARTESIAN_POINT('',(9.395,-0.4,7.));
#22203=CARTESIAN_POINT('Origin',(10.,-0.4,7.));
#22204=CARTESIAN_POINT('Origin',(10.,-0.4,7.));
#22205=CARTESIAN_POINT('',(9.2,0.4,7.));
#22206=CARTESIAN_POINT('Origin',(10.,0.4,7.));
#22207=CARTESIAN_POINT('',(9.2,-0.4,7.));
#22208=CARTESIAN_POINT('',(9.2,-0.4,7.));
#22209=CARTESIAN_POINT('Origin',(10.,-0.4,7.));
#22210=CARTESIAN_POINT('Origin',(10.,0.4,7.));
#22211=CARTESIAN_POINT('Origin',(10.,-0.4,7.));
#22212=CARTESIAN_POINT('',(0.,0.,0.));
#22213=CARTESIAN_POINT('Origin',(10.,-4.,6.));
#22214=CARTESIAN_POINT('',(9.85,-4.,6.4));
#22215=CARTESIAN_POINT('Origin',(10.,-4.,6.4));
#22216=CARTESIAN_POINT('',(9.85,-4.,6.));
#22217=CARTESIAN_POINT('',(9.85,-4.,6.));
#22218=CARTESIAN_POINT('Origin',(10.,-4.,6.));
#22219=CARTESIAN_POINT('Origin',(10.,-4.,6.4));
#22220=CARTESIAN_POINT('Origin',(10.,-4.,6.));
#22221=CARTESIAN_POINT('',(0.,0.,0.));
#22222=CARTESIAN_POINT('Origin',(10.,-4.,7.6));
#22223=CARTESIAN_POINT('',(9.85,-4.,8.));
#22224=CARTESIAN_POINT('Origin',(10.,-4.,8.));
#22225=CARTESIAN_POINT('',(9.85,-4.,7.6));
#22226=CARTESIAN_POINT('',(9.85,-4.,7.6));
#22227=CARTESIAN_POINT('Origin',(10.,-4.,7.6));
#22228=CARTESIAN_POINT('Origin',(10.,-4.,8.));
#22229=CARTESIAN_POINT('Origin',(10.,-4.,7.6));
#22230=CARTESIAN_POINT('',(0.,0.,0.));
#22231=CARTESIAN_POINT('Origin',(10.,-5.2,7.));
#22232=CARTESIAN_POINT('',(9.775,-5.,7.));
#22233=CARTESIAN_POINT('Origin',(10.,-5.,7.));
#22234=CARTESIAN_POINT('',(9.775,-5.2,7.));
#22235=CARTESIAN_POINT('',(9.775,-5.2,7.));
#22236=CARTESIAN_POINT('Origin',(10.,-5.2,7.));
#22237=CARTESIAN_POINT('Origin',(10.,-5.2,7.));
#22238=CARTESIAN_POINT('',(9.2,-5.,7.));
#22239=CARTESIAN_POINT('Origin',(10.,-5.,7.));
#22240=CARTESIAN_POINT('',(9.2,-5.2,7.));
#22241=CARTESIAN_POINT('',(9.2,-5.2,7.));
#22242=CARTESIAN_POINT('Origin',(10.,-5.2,7.));
#22243=CARTESIAN_POINT('Origin',(10.,-5.,7.));
#22244=CARTESIAN_POINT('Origin',(10.,-5.2,7.));
#22245=CARTESIAN_POINT('',(0.,0.,0.));
#22246=CARTESIAN_POINT('Origin',(0.,-0.5,0.));
#22247=CARTESIAN_POINT('',(-1.,-0.375,-6.12323399573677E-17));
#22248=CARTESIAN_POINT('',(-0.992156741649222,-0.5,0.125));
#22249=CARTESIAN_POINT('Ctrl Pts',(-1.,-0.375,-1.00613961606655E-16));
#22250=CARTESIAN_POINT('Ctrl Pts',(-1.,-0.375,0.0157128711428661));
#22251=CARTESIAN_POINT('Ctrl Pts',(-0.999591823858855,-0.378143583103513,
0.0324619190698278));
#22252=CARTESIAN_POINT('Ctrl Pts',(-0.998116453123232,-0.390905426591754,
0.0632545375991437));
#22253=CARTESIAN_POINT('Ctrl Pts',(-0.997070068816062,-0.400522781657727,
0.0772994769543643));
#22254=CARTESIAN_POINT('Ctrl Pts',(-0.995102104277285,-0.422700615683787,
0.0994773109804239));
#22255=CARTESIAN_POINT('Ctrl Pts',(-0.994052129228928,-0.436745514765346,
0.109094593469654));
#22256=CARTESIAN_POINT('Ctrl Pts',(-0.99256853061881,-0.467537996927464,
0.121856383722779));
#22257=CARTESIAN_POINT('Ctrl Pts',(-0.992156741649222,-0.484286997589363,
0.125));
#22258=CARTESIAN_POINT('Ctrl Pts',(-0.992156741649222,-0.5,0.125));
#22259=CARTESIAN_POINT('',(-1.,-0.625,-6.12323399573677E-17));
#22260=CARTESIAN_POINT('Ctrl Pts',(-1.,-0.625,-4.5102810375397E-17));
#22261=CARTESIAN_POINT('Ctrl Pts',(-1.,-0.625,-0.0157128711428662));
#22262=CARTESIAN_POINT('Ctrl Pts',(-0.999591823858855,-0.621856416896487,
-0.032461919069828));
#22263=CARTESIAN_POINT('Ctrl Pts',(-0.998116453123232,-0.609094573408246,
-0.0632545375991439));
#22264=CARTESIAN_POINT('Ctrl Pts',(-0.997070068816062,-0.599477218342273,
-0.0772994769543645));
#22265=CARTESIAN_POINT('Ctrl Pts',(-0.995102104277285,-0.577299384316213,
-0.0994773109804241));
#22266=CARTESIAN_POINT('Ctrl Pts',(-0.994052129228928,-0.563254485234654,
-0.109094593469655));
#22267=CARTESIAN_POINT('Ctrl Pts',(-0.99256853061881,-0.532462003072536,
-0.121856383722779));
#22268=CARTESIAN_POINT('Ctrl Pts',(-0.992156741649221,-0.515713002410637,
-0.125));
#22269=CARTESIAN_POINT('Ctrl Pts',(-0.992156741649221,-0.484286997589363,
-0.125));
#22270=CARTESIAN_POINT('Ctrl Pts',(-0.99256853061881,-0.467537996927464,
-0.121856383722779));
#22271=CARTESIAN_POINT('Ctrl Pts',(-0.994052129228928,-0.436745514765346,
-0.109094593469655));
#22272=CARTESIAN_POINT('Ctrl Pts',(-0.995102104277285,-0.422700615683787,
-0.0994773109804241));
#22273=CARTESIAN_POINT('Ctrl Pts',(-0.997070068816062,-0.400522781657728,
-0.0772994769543645));
#22274=CARTESIAN_POINT('Ctrl Pts',(-0.998116453123232,-0.390905426591754,
-0.063254537599144));
#22275=CARTESIAN_POINT('Ctrl Pts',(-0.999591823858855,-0.378143583103513,
-0.0324619190698281));
#22276=CARTESIAN_POINT('Ctrl Pts',(-1.,-0.375,-0.0157128711428663));
#22277=CARTESIAN_POINT('Ctrl Pts',(-1.,-0.375,-9.36750677027476E-17));
#22278=CARTESIAN_POINT('Ctrl Pts',(-0.992156741649222,-0.5,0.125));
#22279=CARTESIAN_POINT('Ctrl Pts',(-0.992156741649222,-0.515713002410637,
0.125));
#22280=CARTESIAN_POINT('Ctrl Pts',(-0.99256853061881,-0.532462003072536,
0.121856383722779));
#22281=CARTESIAN_POINT('Ctrl Pts',(-0.994052129228928,-0.563254485234654,
0.109094593469654));
#22282=CARTESIAN_POINT('Ctrl Pts',(-0.995102104277285,-0.577299384316213,
0.0994773109804241));
#22283=CARTESIAN_POINT('Ctrl Pts',(-0.997070068816062,-0.599477218342273,
0.0772994769543644));
#22284=CARTESIAN_POINT('Ctrl Pts',(-0.998116453123232,-0.609094573408246,
0.0632545375991438));
#22285=CARTESIAN_POINT('Ctrl Pts',(-0.999591823858855,-0.621856416896487,
0.0324619190698279));
#22286=CARTESIAN_POINT('Ctrl Pts',(-1.,-0.625,0.0157128711428661));
#22287=CARTESIAN_POINT('Ctrl Pts',(-1.,-0.625,-4.85722573273506E-17));
#22288=CARTESIAN_POINT('',(-0.586834729715275,-0.5,0.125));
#22289=CARTESIAN_POINT('',(-7.65404249467096E-18,-0.5,0.125));
#22290=CARTESIAN_POINT('',(-0.6,-0.625,1.24532753107453E-17));
#22291=CARTESIAN_POINT('Ctrl Pts',(-0.6,-0.625,-4.16333634234434E-17));
#22292=CARTESIAN_POINT('Ctrl Pts',(-0.6,-0.625,0.0157444828659572));
#22293=CARTESIAN_POINT('Ctrl Pts',(-0.599317707212167,-0.621844041497889,
0.0325072544867633));
#22294=CARTESIAN_POINT('Ctrl Pts',(-0.596852269967858,-0.609072857638709,
0.0632914182239686));
#22295=CARTESIAN_POINT('Ctrl Pts',(-0.59510289473619,-0.599460146728784,
0.077316548567853));
#22296=CARTESIAN_POINT('Ctrl Pts',(-0.591804743154611,-0.577315815675743,
0.0994608796208941));
#22297=CARTESIAN_POINT('Ctrl Pts',(-0.590038488226116,-0.563290995658393,
0.109073016834181));
#22298=CARTESIAN_POINT('Ctrl Pts',(-0.587534197873268,-0.532507913768158,
0.121843784097853));
#22299=CARTESIAN_POINT('Ctrl Pts',(-0.586834729715275,-0.515745525063995,
0.125));
#22300=CARTESIAN_POINT('Ctrl Pts',(-0.586834729715275,-0.5,0.125));
#22301=CARTESIAN_POINT('',(-0.586834729715275,-0.5,-0.125));
#22302=CARTESIAN_POINT('Ctrl Pts',(-0.586834729715275,-0.5,-0.125));
#22303=CARTESIAN_POINT('Ctrl Pts',(-0.586834729715275,-0.515745525063995,
-0.125));
#22304=CARTESIAN_POINT('Ctrl Pts',(-0.587534197873268,-0.532507913768158,
-0.121843784097853));
#22305=CARTESIAN_POINT('Ctrl Pts',(-0.590038488226116,-0.563290995658393,
-0.109073016834181));
#22306=CARTESIAN_POINT('Ctrl Pts',(-0.591804743154611,-0.577315815675743,
-0.0994608796208942));
#22307=CARTESIAN_POINT('Ctrl Pts',(-0.59510289473619,-0.599460146728784,
-0.0773165485678531));
#22308=CARTESIAN_POINT('Ctrl Pts',(-0.596852269967858,-0.609072857638709,
-0.0632914182239687));
#22309=CARTESIAN_POINT('Ctrl Pts',(-0.599317707212167,-0.621844041497889,
-0.0325072544867635));
#22310=CARTESIAN_POINT('Ctrl Pts',(-0.6,-0.625,-0.0157444828659573));
#22311=CARTESIAN_POINT('Ctrl Pts',(-0.6,-0.625,-5.20417042793042E-17));
#22312=CARTESIAN_POINT('',(-0.6,-0.375,3.50046804984438E-17));
#22313=CARTESIAN_POINT('Ctrl Pts',(-0.6,-0.375,-3.46944695195361E-18));
#22314=CARTESIAN_POINT('Ctrl Pts',(-0.6,-0.375,-0.0157444828659572));
#22315=CARTESIAN_POINT('Ctrl Pts',(-0.599317707212167,-0.378155958502111,
-0.0325072544867634));
#22316=CARTESIAN_POINT('Ctrl Pts',(-0.596852269967858,-0.390927142361291,
-0.0632914182239686));
#22317=CARTESIAN_POINT('Ctrl Pts',(-0.59510289473619,-0.400539853271216,
-0.077316548567853));
#22318=CARTESIAN_POINT('Ctrl Pts',(-0.591804743154611,-0.422684184324257,
-0.0994608796208942));
#22319=CARTESIAN_POINT('Ctrl Pts',(-0.590038488226116,-0.436709004341607,
-0.109073016834181));
#22320=CARTESIAN_POINT('Ctrl Pts',(-0.587534197873268,-0.467492086231842,
-0.121843784097853));
#22321=CARTESIAN_POINT('Ctrl Pts',(-0.586834729715275,-0.484254474936005,
-0.125));
#22322=CARTESIAN_POINT('Ctrl Pts',(-0.586834729715275,-0.5,-0.125));
#22323=CARTESIAN_POINT('Ctrl Pts',(-0.586834729715275,-0.5,0.125));
#22324=CARTESIAN_POINT('Ctrl Pts',(-0.586834729715275,-0.484254474936005,
0.125));
#22325=CARTESIAN_POINT('Ctrl Pts',(-0.587534197873268,-0.467492086231842,
0.121843784097853));
#22326=CARTESIAN_POINT('Ctrl Pts',(-0.590038488226116,-0.436709004341607,
0.109073016834181));
#22327=CARTESIAN_POINT('Ctrl Pts',(-0.591804743154611,-0.422684184324257,
0.0994608796208941));
#22328=CARTESIAN_POINT('Ctrl Pts',(-0.59510289473619,-0.400539853271216,
0.077316548567853));
#22329=CARTESIAN_POINT('Ctrl Pts',(-0.596852269967858,-0.390927142361291,
0.0632914182239686));
#22330=CARTESIAN_POINT('Ctrl Pts',(-0.599317707212167,-0.378155958502111,
0.0325072544867634));
#22331=CARTESIAN_POINT('Ctrl Pts',(-0.6,-0.375,0.0157444828659572));
#22332=CARTESIAN_POINT('Ctrl Pts',(-0.6,-0.375,-2.42861286636753E-17));
#22333=CARTESIAN_POINT('Origin',(0.,-0.5,0.));
#22334=CARTESIAN_POINT('',(0.586834729715275,-0.5,-0.125));
#22335=CARTESIAN_POINT('',(0.586834729715275,-0.5,0.125));
#22336=CARTESIAN_POINT('Ctrl Pts',(0.586834729715275,-0.5,-0.125));
#22337=CARTESIAN_POINT('Ctrl Pts',(0.586834729715275,-0.484254474936005,
-0.125));
#22338=CARTESIAN_POINT('Ctrl Pts',(0.587534197873268,-0.467492086231842,
-0.121843784097853));
#22339=CARTESIAN_POINT('Ctrl Pts',(0.590038488226116,-0.436709004341607,
-0.109073016834181));
#22340=CARTESIAN_POINT('Ctrl Pts',(0.591804743154611,-0.422684184324257,
-0.0994608796208941));
#22341=CARTESIAN_POINT('Ctrl Pts',(0.59510289473619,-0.400539853271216,
-0.0773165485678529));
#22342=CARTESIAN_POINT('Ctrl Pts',(0.596852269967858,-0.390927142361291,
-0.0632914182239686));
#22343=CARTESIAN_POINT('Ctrl Pts',(0.599317707212167,-0.378155958502111,
-0.0325072544867633));
#22344=CARTESIAN_POINT('Ctrl Pts',(0.6,-0.375,-0.0157444828659572));
#22345=CARTESIAN_POINT('Ctrl Pts',(0.6,-0.375,0.0157444828659573));
#22346=CARTESIAN_POINT('Ctrl Pts',(0.599317707212167,-0.378155958502111,
0.0325072544867635));
#22347=CARTESIAN_POINT('Ctrl Pts',(0.596852269967858,-0.390927142361291,
0.0632914182239687));
#22348=CARTESIAN_POINT('Ctrl Pts',(0.59510289473619,-0.400539853271216,
0.0773165485678531));
#22349=CARTESIAN_POINT('Ctrl Pts',(0.591804743154611,-0.422684184324257,
0.0994608796208942));
#22350=CARTESIAN_POINT('Ctrl Pts',(0.590038488226116,-0.436709004341607,
0.109073016834181));
#22351=CARTESIAN_POINT('Ctrl Pts',(0.587534197873268,-0.467492086231842,
0.121843784097853));
#22352=CARTESIAN_POINT('Ctrl Pts',(0.586834729715275,-0.484254474936005,
0.125));
#22353=CARTESIAN_POINT('Ctrl Pts',(0.586834729715275,-0.5,0.125));
#22354=CARTESIAN_POINT('Ctrl Pts',(0.586834729715275,-0.5,0.125));
#22355=CARTESIAN_POINT('Ctrl Pts',(0.586834729715275,-0.515745525063995,
0.125));
#22356=CARTESIAN_POINT('Ctrl Pts',(0.587534197873268,-0.532507913768158,
0.121843784097853));
#22357=CARTESIAN_POINT('Ctrl Pts',(0.590038488226116,-0.563290995658393,
0.109073016834181));
#22358=CARTESIAN_POINT('Ctrl Pts',(0.591804743154611,-0.577315815675743,
0.0994608796208942));
#22359=CARTESIAN_POINT('Ctrl Pts',(0.59510289473619,-0.599460146728784,
0.077316548567853));
#22360=CARTESIAN_POINT('Ctrl Pts',(0.596852269967858,-0.609072857638709,
0.0632914182239688));
#22361=CARTESIAN_POINT('Ctrl Pts',(0.599317707212167,-0.621844041497889,
0.0325072544867635));
#22362=CARTESIAN_POINT('Ctrl Pts',(0.6,-0.625,0.0157444828659573));
#22363=CARTESIAN_POINT('Ctrl Pts',(0.6,-0.625,-0.0157444828659572));
#22364=CARTESIAN_POINT('Ctrl Pts',(0.599317707212167,-0.621844041497889,
-0.0325072544867633));
#22365=CARTESIAN_POINT('Ctrl Pts',(0.596852269967858,-0.609072857638709,
-0.0632914182239685));
#22366=CARTESIAN_POINT('Ctrl Pts',(0.59510289473619,-0.599460146728784,
-0.077316548567853));
#22367=CARTESIAN_POINT('Ctrl Pts',(0.591804743154611,-0.577315815675743,
-0.0994608796208941));
#22368=CARTESIAN_POINT('Ctrl Pts',(0.590038488226116,-0.563290995658393,
-0.10907301683418));
#22369=CARTESIAN_POINT('Ctrl Pts',(0.587534197873268,-0.532507913768158,
-0.121843784097853));
#22370=CARTESIAN_POINT('Ctrl Pts',(0.586834729715275,-0.515745525063995,
-0.125));
#22371=CARTESIAN_POINT('Ctrl Pts',(0.586834729715275,-0.5,-0.125));
#22372=CARTESIAN_POINT('',(0.992156741649222,-0.5,0.125));
#22373=CARTESIAN_POINT('',(-7.65404249467096E-18,-0.5,0.125));
#22374=CARTESIAN_POINT('',(1.,-0.625,6.12323399573677E-17));
#22375=CARTESIAN_POINT('Ctrl Pts',(1.,-0.625,7.28583859910259E-17));
#22376=CARTESIAN_POINT('Ctrl Pts',(1.,-0.625,0.0157128711428663));
#22377=CARTESIAN_POINT('Ctrl Pts',(0.999591823858855,-0.621856416896487,
0.032461919069828));
#22378=CARTESIAN_POINT('Ctrl Pts',(0.998116453123232,-0.609094573408246,
0.0632545375991439));
#22379=CARTESIAN_POINT('Ctrl Pts',(0.997070068816062,-0.599477218342273,
0.0772994769543645));
#22380=CARTESIAN_POINT('Ctrl Pts',(0.995102104277285,-0.577299384316213,
0.0994773109804242));
#22381=CARTESIAN_POINT('Ctrl Pts',(0.994052129228928,-0.563254485234654,
0.109094593469655));
#22382=CARTESIAN_POINT('Ctrl Pts',(0.99256853061881,-0.532462003072536,
0.121856383722779));
#22383=CARTESIAN_POINT('Ctrl Pts',(0.992156741649222,-0.515713002410637,
0.125));
#22384=CARTESIAN_POINT('Ctrl Pts',(0.992156741649222,-0.5,0.125));
#22385=CARTESIAN_POINT('',(1.,-0.375,6.12323399573677E-17));
#22386=CARTESIAN_POINT('Ctrl Pts',(1.,-0.375,2.08166817117217E-17));
#22387=CARTESIAN_POINT('Ctrl Pts',(1.,-0.375,-0.0157128711428662));
#22388=CARTESIAN_POINT('Ctrl Pts',(0.999591823858855,-0.378143583103513,
-0.032461919069828));
#22389=CARTESIAN_POINT('Ctrl Pts',(0.998116453123232,-0.390905426591754,
-0.0632545375991438));
#22390=CARTESIAN_POINT('Ctrl Pts',(0.997070068816062,-0.400522781657728,
-0.0772994769543644));
#22391=CARTESIAN_POINT('Ctrl Pts',(0.995102104277285,-0.422700615683787,
-0.099477310980424));
#22392=CARTESIAN_POINT('Ctrl Pts',(0.994052129228928,-0.436745514765346,
-0.109094593469654));
#22393=CARTESIAN_POINT('Ctrl Pts',(0.99256853061881,-0.467537996927464,
-0.121856383722779));
#22394=CARTESIAN_POINT('Ctrl Pts',(0.992156741649222,-0.484286997589363,
-0.125));
#22395=CARTESIAN_POINT('Ctrl Pts',(0.992156741649222,-0.515713002410637,
-0.125));
#22396=CARTESIAN_POINT('Ctrl Pts',(0.99256853061881,-0.532462003072536,
-0.121856383722779));
#22397=CARTESIAN_POINT('Ctrl Pts',(0.994052129228928,-0.563254485234654,
-0.109094593469654));
#22398=CARTESIAN_POINT('Ctrl Pts',(0.995102104277285,-0.577299384316213,
-0.099477310980424));
#22399=CARTESIAN_POINT('Ctrl Pts',(0.997070068816062,-0.599477218342273,
-0.0772994769543643));
#22400=CARTESIAN_POINT('Ctrl Pts',(0.998116453123232,-0.609094573408246,
-0.0632545375991438));
#22401=CARTESIAN_POINT('Ctrl Pts',(0.999591823858855,-0.621856416896487,
-0.0324619190698279));
#22402=CARTESIAN_POINT('Ctrl Pts',(1.,-0.625,-0.0157128711428661));
#22403=CARTESIAN_POINT('Ctrl Pts',(1.,-0.625,8.32667268468867E-17));
#22404=CARTESIAN_POINT('Ctrl Pts',(0.992156741649222,-0.5,0.125));
#22405=CARTESIAN_POINT('Ctrl Pts',(0.992156741649222,-0.484286997589363,
0.125));
#22406=CARTESIAN_POINT('Ctrl Pts',(0.99256853061881,-0.467537996927464,
0.121856383722779));
#22407=CARTESIAN_POINT('Ctrl Pts',(0.994052129228928,-0.436745514765346,
0.109094593469654));
#22408=CARTESIAN_POINT('Ctrl Pts',(0.995102104277285,-0.422700615683787,
0.0994773109804241));
#22409=CARTESIAN_POINT('Ctrl Pts',(0.997070068816062,-0.400522781657727,
0.0772994769543644));
#22410=CARTESIAN_POINT('Ctrl Pts',(0.998116453123232,-0.390905426591754,
0.0632545375991438));
#22411=CARTESIAN_POINT('Ctrl Pts',(0.999591823858855,-0.378143583103513,
0.0324619190698279));
#22412=CARTESIAN_POINT('Ctrl Pts',(1.,-0.375,0.0157128711428662));
#22413=CARTESIAN_POINT('Ctrl Pts',(1.,-0.375,2.77555756156289E-17));
#22414=CARTESIAN_POINT('Origin',(0.,-0.1,0.));
#22415=CARTESIAN_POINT('',(-1.,-0.9,1.22464679914735E-16));
#22416=CARTESIAN_POINT('Origin',(0.,-0.9,0.));
#22417=CARTESIAN_POINT('',(-1.,-0.1,-1.22464679914735E-16));
#22418=CARTESIAN_POINT('',(-1.,-0.1,1.22464679914735E-16));
#22419=CARTESIAN_POINT('',(-1.,-0.1,-1.22464679914735E-16));
#22420=CARTESIAN_POINT('Origin',(0.,-0.1,0.));
#22421=CARTESIAN_POINT('',(0.,-0.625,-1.));
#22422=CARTESIAN_POINT('',(0.,-0.375,-1.));
#22423=CARTESIAN_POINT('Ctrl Pts',(-2.08166817117217E-17,-0.625,-1.));
#22424=CARTESIAN_POINT('Ctrl Pts',(0.0157128711428662,-0.625,-1.));
#22425=CARTESIAN_POINT('Ctrl Pts',(0.0324619190698279,-0.621856416896487,
-0.999591823858855));
#22426=CARTESIAN_POINT('Ctrl Pts',(0.0632545375991438,-0.609094573408246,
-0.998116453123232));
#22427=CARTESIAN_POINT('Ctrl Pts',(0.0772994769543644,-0.599477218342273,
-0.997070068816062));
#22428=CARTESIAN_POINT('Ctrl Pts',(0.0994773109804241,-0.577299384316213,
-0.995102104277285));
#22429=CARTESIAN_POINT('Ctrl Pts',(0.109094593469654,-0.563254485234654,
-0.994052129228928));
#22430=CARTESIAN_POINT('Ctrl Pts',(0.121856383722779,-0.532462003072536,
-0.99256853061881));
#22431=CARTESIAN_POINT('Ctrl Pts',(0.125,-0.515713002410637,-0.992156741649221));
#22432=CARTESIAN_POINT('Ctrl Pts',(0.125,-0.484286997589363,-0.992156741649221));
#22433=CARTESIAN_POINT('Ctrl Pts',(0.121856383722779,-0.467537996927464,
-0.99256853061881));
#22434=CARTESIAN_POINT('Ctrl Pts',(0.109094593469654,-0.436745514765346,
-0.994052129228928));
#22435=CARTESIAN_POINT('Ctrl Pts',(0.0994773109804241,-0.422700615683787,
-0.995102104277285));
#22436=CARTESIAN_POINT('Ctrl Pts',(0.0772994769543645,-0.400522781657728,
-0.997070068816062));
#22437=CARTESIAN_POINT('Ctrl Pts',(0.0632545375991439,-0.390905426591754,
-0.998116453123232));
#22438=CARTESIAN_POINT('Ctrl Pts',(0.032461919069828,-0.378143583103513,
-0.999591823858855));
#22439=CARTESIAN_POINT('Ctrl Pts',(0.0157128711428662,-0.375,-1.));
#22440=CARTESIAN_POINT('Ctrl Pts',(3.81639164714898E-17,-0.375,-1.));
#22441=CARTESIAN_POINT('',(-0.125,-0.5,-0.992156741649222));
#22442=CARTESIAN_POINT('Ctrl Pts',(4.5102810375397E-17,-0.375,-1.));
#22443=CARTESIAN_POINT('Ctrl Pts',(-0.0157128711428661,-0.375,-1.));
#22444=CARTESIAN_POINT('Ctrl Pts',(-0.0324619190698279,-0.378143583103513,
-0.999591823858855));
#22445=CARTESIAN_POINT('Ctrl Pts',(-0.0632545375991437,-0.390905426591754,
-0.998116453123232));
#22446=CARTESIAN_POINT('Ctrl Pts',(-0.0772994769543643,-0.400522781657727,
-0.997070068816062));
#22447=CARTESIAN_POINT('Ctrl Pts',(-0.099477310980424,-0.422700615683787,
-0.995102104277285));
#22448=CARTESIAN_POINT('Ctrl Pts',(-0.109094593469654,-0.436745514765346,
-0.994052129228928));
#22449=CARTESIAN_POINT('Ctrl Pts',(-0.121856383722779,-0.467537996927464,
-0.99256853061881));
#22450=CARTESIAN_POINT('Ctrl Pts',(-0.125,-0.484286997589363,-0.992156741649222));
#22451=CARTESIAN_POINT('Ctrl Pts',(-0.125,-0.5,-0.992156741649222));
#22452=CARTESIAN_POINT('Ctrl Pts',(-0.125,-0.5,-0.992156741649222));
#22453=CARTESIAN_POINT('Ctrl Pts',(-0.125,-0.515713002410637,-0.992156741649222));
#22454=CARTESIAN_POINT('Ctrl Pts',(-0.121856383722779,-0.532462003072536,
-0.99256853061881));
#22455=CARTESIAN_POINT('Ctrl Pts',(-0.109094593469654,-0.563254485234654,
-0.994052129228928));
#22456=CARTESIAN_POINT('Ctrl Pts',(-0.0994773109804241,-0.577299384316213,
-0.995102104277285));
#22457=CARTESIAN_POINT('Ctrl Pts',(-0.0772994769543644,-0.599477218342273,
-0.997070068816062));
#22458=CARTESIAN_POINT('Ctrl Pts',(-0.0632545375991439,-0.609094573408246,
-0.998116453123232));
#22459=CARTESIAN_POINT('Ctrl Pts',(-0.032461919069828,-0.621856416896487,
-0.999591823858855));
#22460=CARTESIAN_POINT('Ctrl Pts',(-0.0157128711428662,-0.625,-1.));
#22461=CARTESIAN_POINT('Ctrl Pts',(-1.38777878078145E-17,-0.625,-1.));
#22462=CARTESIAN_POINT('',(0.,-0.375,1.));
#22463=CARTESIAN_POINT('',(0.,-0.625,1.));
#22464=CARTESIAN_POINT('Ctrl Pts',(4.16333634234434E-17,-0.375,1.));
#22465=CARTESIAN_POINT('Ctrl Pts',(0.0157128711428662,-0.375,1.));
#22466=CARTESIAN_POINT('Ctrl Pts',(0.032461919069828,-0.378143583103513,
0.999591823858855));
#22467=CARTESIAN_POINT('Ctrl Pts',(0.0632545375991439,-0.390905426591754,
0.998116453123232));
#22468=CARTESIAN_POINT('Ctrl Pts',(0.0772994769543644,-0.400522781657728,
0.997070068816062));
#22469=CARTESIAN_POINT('Ctrl Pts',(0.0994773109804241,-0.422700615683787,
0.995102104277285));
#22470=CARTESIAN_POINT('Ctrl Pts',(0.109094593469654,-0.436745514765346,
0.994052129228928));
#22471=CARTESIAN_POINT('Ctrl Pts',(0.121856383722779,-0.467537996927464,
0.99256853061881));
#22472=CARTESIAN_POINT('Ctrl Pts',(0.125,-0.484286997589363,0.992156741649222));
#22473=CARTESIAN_POINT('Ctrl Pts',(0.125,-0.515713002410637,0.992156741649222));
#22474=CARTESIAN_POINT('Ctrl Pts',(0.121856383722779,-0.532462003072536,
0.99256853061881));
#22475=CARTESIAN_POINT('Ctrl Pts',(0.109094593469655,-0.563254485234654,
0.994052129228928));
#22476=CARTESIAN_POINT('Ctrl Pts',(0.0994773109804241,-0.577299384316213,
0.995102104277285));
#22477=CARTESIAN_POINT('Ctrl Pts',(0.0772994769543644,-0.599477218342273,
0.997070068816062));
#22478=CARTESIAN_POINT('Ctrl Pts',(0.0632545375991438,-0.609094573408246,
0.998116453123232));
#22479=CARTESIAN_POINT('Ctrl Pts',(0.0324619190698279,-0.621856416896487,
0.999591823858855));
#22480=CARTESIAN_POINT('Ctrl Pts',(0.0157128711428662,-0.625,1.));
#22481=CARTESIAN_POINT('Ctrl Pts',(-1.73472347597681E-17,-0.625,1.));
#22482=CARTESIAN_POINT('',(-0.125,-0.5,0.992156741649222));
#22483=CARTESIAN_POINT('Ctrl Pts',(-1.73472347597681E-17,-0.625,1.));
#22484=CARTESIAN_POINT('Ctrl Pts',(-0.0157128711428662,-0.625,1.));
#22485=CARTESIAN_POINT('Ctrl Pts',(-0.032461919069828,-0.621856416896487,
0.999591823858855));
#22486=CARTESIAN_POINT('Ctrl Pts',(-0.0632545375991439,-0.609094573408246,
0.998116453123232));
#22487=CARTESIAN_POINT('Ctrl Pts',(-0.0772994769543645,-0.599477218342273,
0.997070068816062));
#22488=CARTESIAN_POINT('Ctrl Pts',(-0.0994773109804241,-0.577299384316213,
0.995102104277285));
#22489=CARTESIAN_POINT('Ctrl Pts',(-0.109094593469654,-0.563254485234654,
0.994052129228928));
#22490=CARTESIAN_POINT('Ctrl Pts',(-0.121856383722779,-0.532462003072536,
0.99256853061881));
#22491=CARTESIAN_POINT('Ctrl Pts',(-0.125,-0.515713002410637,0.992156741649222));
#22492=CARTESIAN_POINT('Ctrl Pts',(-0.125,-0.5,0.992156741649222));
#22493=CARTESIAN_POINT('Ctrl Pts',(-0.125,-0.5,0.992156741649222));
#22494=CARTESIAN_POINT('Ctrl Pts',(-0.125,-0.484286997589363,0.992156741649222));
#22495=CARTESIAN_POINT('Ctrl Pts',(-0.121856383722779,-0.467537996927464,
0.99256853061881));
#22496=CARTESIAN_POINT('Ctrl Pts',(-0.109094593469654,-0.436745514765346,
0.994052129228928));
#22497=CARTESIAN_POINT('Ctrl Pts',(-0.099477310980424,-0.422700615683787,
0.995102104277285));
#22498=CARTESIAN_POINT('Ctrl Pts',(-0.0772994769543643,-0.400522781657727,
0.997070068816062));
#22499=CARTESIAN_POINT('Ctrl Pts',(-0.0632545375991438,-0.390905426591754,
0.998116453123232));
#22500=CARTESIAN_POINT('Ctrl Pts',(-0.0324619190698279,-0.378143583103513,
0.999591823858855));
#22501=CARTESIAN_POINT('Ctrl Pts',(-0.0157128711428661,-0.375,1.));
#22502=CARTESIAN_POINT('Ctrl Pts',(4.5102810375397E-17,-0.375,1.));
#22503=CARTESIAN_POINT('Origin',(0.,-0.5,0.));
#22504=CARTESIAN_POINT('',(-0.125,-0.5,-0.586834729715275));
#22505=CARTESIAN_POINT('',(-0.125,-0.5,0.));
#22506=CARTESIAN_POINT('',(0.125,-0.5,-0.586834729715275));
#22507=CARTESIAN_POINT('Ctrl Pts',(0.125,-0.5,-0.586834729715275));
#22508=CARTESIAN_POINT('Ctrl Pts',(0.125,-0.515745525063995,-0.586834729715275));
#22509=CARTESIAN_POINT('Ctrl Pts',(0.121843784097853,-0.532507913768158,
-0.587534197873268));
#22510=CARTESIAN_POINT('Ctrl Pts',(0.109073016834181,-0.563290995658393,
-0.590038488226116));
#22511=CARTESIAN_POINT('Ctrl Pts',(0.0994608796208942,-0.577315815675743,
-0.591804743154611));
#22512=CARTESIAN_POINT('Ctrl Pts',(0.077316548567853,-0.599460146728784,
-0.59510289473619));
#22513=CARTESIAN_POINT('Ctrl Pts',(0.0632914182239686,-0.609072857638709,
-0.596852269967858));
#22514=CARTESIAN_POINT('Ctrl Pts',(0.0325072544867633,-0.621844041497889,
-0.599317707212167));
#22515=CARTESIAN_POINT('Ctrl Pts',(0.0157444828659573,-0.625,-0.6));
#22516=CARTESIAN_POINT('Ctrl Pts',(-0.0157444828659572,-0.625,-0.6));
#22517=CARTESIAN_POINT('Ctrl Pts',(-0.0325072544867633,-0.621844041497889,
-0.599317707212167));
#22518=CARTESIAN_POINT('Ctrl Pts',(-0.0632914182239686,-0.609072857638709,
-0.596852269967858));
#22519=CARTESIAN_POINT('Ctrl Pts',(-0.077316548567853,-0.599460146728784,
-0.59510289473619));
#22520=CARTESIAN_POINT('Ctrl Pts',(-0.0994608796208941,-0.577315815675743,
-0.591804743154611));
#22521=CARTESIAN_POINT('Ctrl Pts',(-0.109073016834181,-0.563290995658393,
-0.590038488226116));
#22522=CARTESIAN_POINT('Ctrl Pts',(-0.121843784097853,-0.532507913768158,
-0.587534197873268));
#22523=CARTESIAN_POINT('Ctrl Pts',(-0.125,-0.515745525063995,-0.586834729715275));
#22524=CARTESIAN_POINT('Ctrl Pts',(-0.125,-0.5,-0.586834729715275));
#22525=CARTESIAN_POINT('Ctrl Pts',(-0.125,-0.5,-0.586834729715275));
#22526=CARTESIAN_POINT('Ctrl Pts',(-0.125,-0.484254474936005,-0.586834729715275));
#22527=CARTESIAN_POINT('Ctrl Pts',(-0.121843784097853,-0.467492086231842,
-0.587534197873268));
#22528=CARTESIAN_POINT('Ctrl Pts',(-0.109073016834181,-0.436709004341607,
-0.590038488226116));
#22529=CARTESIAN_POINT('Ctrl Pts',(-0.0994608796208942,-0.422684184324257,
-0.591804743154611));
#22530=CARTESIAN_POINT('Ctrl Pts',(-0.077316548567853,-0.400539853271216,
-0.59510289473619));
#22531=CARTESIAN_POINT('Ctrl Pts',(-0.0632914182239687,-0.39092714236129,
-0.596852269967858));
#22532=CARTESIAN_POINT('Ctrl Pts',(-0.0325072544867634,-0.378155958502111,
-0.599317707212167));
#22533=CARTESIAN_POINT('Ctrl Pts',(-0.0157444828659573,-0.375,-0.6));
#22534=CARTESIAN_POINT('Ctrl Pts',(0.0157444828659572,-0.375,-0.6));
#22535=CARTESIAN_POINT('Ctrl Pts',(0.0325072544867634,-0.378155958502111,
-0.599317707212167));
#22536=CARTESIAN_POINT('Ctrl Pts',(0.0632914182239686,-0.390927142361291,
-0.596852269967858));
#22537=CARTESIAN_POINT('Ctrl Pts',(0.077316548567853,-0.400539853271216,
-0.59510289473619));
#22538=CARTESIAN_POINT('Ctrl Pts',(0.0994608796208941,-0.422684184324257,
-0.591804743154611));
#22539=CARTESIAN_POINT('Ctrl Pts',(0.109073016834181,-0.436709004341607,
-0.590038488226116));
#22540=CARTESIAN_POINT('Ctrl Pts',(0.121843784097853,-0.467492086231842,
-0.587534197873268));
#22541=CARTESIAN_POINT('Ctrl Pts',(0.125,-0.484254474936005,-0.586834729715275));
#22542=CARTESIAN_POINT('Ctrl Pts',(0.125,-0.5,-0.586834729715275));
#22543=CARTESIAN_POINT('Origin',(0.,-0.5,0.));
#22544=CARTESIAN_POINT('',(0.125,-0.5,0.586834729715275));
#22545=CARTESIAN_POINT('',(-0.125,-0.5,0.586834729715275));
#22546=CARTESIAN_POINT('Ctrl Pts',(0.125,-0.5,0.586834729715275));
#22547=CARTESIAN_POINT('Ctrl Pts',(0.125,-0.484254474936005,0.586834729715275));
#22548=CARTESIAN_POINT('Ctrl Pts',(0.121843784097853,-0.467492086231842,
0.587534197873268));
#22549=CARTESIAN_POINT('Ctrl Pts',(0.109073016834181,-0.436709004341607,
0.590038488226116));
#22550=CARTESIAN_POINT('Ctrl Pts',(0.0994608796208941,-0.422684184324257,
0.591804743154611));
#22551=CARTESIAN_POINT('Ctrl Pts',(0.077316548567853,-0.400539853271216,
0.59510289473619));
#22552=CARTESIAN_POINT('Ctrl Pts',(0.0632914182239686,-0.390927142361291,
0.596852269967858));
#22553=CARTESIAN_POINT('Ctrl Pts',(0.0325072544867634,-0.378155958502111,
0.599317707212167));
#22554=CARTESIAN_POINT('Ctrl Pts',(0.0157444828659572,-0.375,0.6));
#22555=CARTESIAN_POINT('Ctrl Pts',(-0.0157444828659573,-0.375,0.6));
#22556=CARTESIAN_POINT('Ctrl Pts',(-0.0325072544867634,-0.378155958502111,
0.599317707212167));
#22557=CARTESIAN_POINT('Ctrl Pts',(-0.0632914182239687,-0.390927142361291,
0.596852269967858));
#22558=CARTESIAN_POINT('Ctrl Pts',(-0.077316548567853,-0.400539853271216,
0.59510289473619));
#22559=CARTESIAN_POINT('Ctrl Pts',(-0.0994608796208942,-0.422684184324257,
0.591804743154611));
#22560=CARTESIAN_POINT('Ctrl Pts',(-0.109073016834181,-0.436709004341607,
0.590038488226116));
#22561=CARTESIAN_POINT('Ctrl Pts',(-0.121843784097853,-0.467492086231842,
0.587534197873268));
#22562=CARTESIAN_POINT('Ctrl Pts',(-0.125,-0.484254474936005,0.586834729715275));
#22563=CARTESIAN_POINT('Ctrl Pts',(-0.125,-0.5,0.586834729715275));
#22564=CARTESIAN_POINT('Ctrl Pts',(-0.125,-0.5,0.586834729715275));
#22565=CARTESIAN_POINT('Ctrl Pts',(-0.125,-0.515745525063995,0.586834729715275));
#22566=CARTESIAN_POINT('Ctrl Pts',(-0.121843784097853,-0.532507913768158,
0.587534197873268));
#22567=CARTESIAN_POINT('Ctrl Pts',(-0.109073016834181,-0.563290995658393,
0.590038488226116));
#22568=CARTESIAN_POINT('Ctrl Pts',(-0.0994608796208941,-0.577315815675743,
0.591804743154611));
#22569=CARTESIAN_POINT('Ctrl Pts',(-0.077316548567853,-0.599460146728784,
0.59510289473619));
#22570=CARTESIAN_POINT('Ctrl Pts',(-0.0632914182239687,-0.609072857638709,
0.596852269967858));
#22571=CARTESIAN_POINT('Ctrl Pts',(-0.0325072544867635,-0.621844041497889,
0.599317707212167));
#22572=CARTESIAN_POINT('Ctrl Pts',(-0.0157444828659572,-0.625,0.6));
#22573=CARTESIAN_POINT('Ctrl Pts',(0.0157444828659572,-0.625,0.6));
#22574=CARTESIAN_POINT('Ctrl Pts',(0.0325072544867633,-0.621844041497889,
0.599317707212167));
#22575=CARTESIAN_POINT('Ctrl Pts',(0.0632914182239686,-0.609072857638709,
0.596852269967858));
#22576=CARTESIAN_POINT('Ctrl Pts',(0.077316548567853,-0.599460146728784,
0.59510289473619));
#22577=CARTESIAN_POINT('Ctrl Pts',(0.0994608796208942,-0.577315815675743,
0.591804743154611));
#22578=CARTESIAN_POINT('Ctrl Pts',(0.109073016834181,-0.563290995658393,
0.590038488226116));
#22579=CARTESIAN_POINT('Ctrl Pts',(0.121843784097853,-0.532507913768158,
0.587534197873268));
#22580=CARTESIAN_POINT('Ctrl Pts',(0.125,-0.515745525063995,0.586834729715275));
#22581=CARTESIAN_POINT('Ctrl Pts',(0.125,-0.5,0.586834729715275));
#22582=CARTESIAN_POINT('',(-0.125,-0.5,0.));
#22583=CARTESIAN_POINT('Origin',(0.,0.,0.));
#22584=CARTESIAN_POINT('',(-0.6,-0.9,7.34788079488412E-17));
#22585=CARTESIAN_POINT('Origin',(0.,-0.9,0.));
#22586=CARTESIAN_POINT('',(-0.6,0.,7.34788079488412E-17));
#22587=CARTESIAN_POINT('',(-0.6,0.85,-7.34788079488412E-17));
#22588=CARTESIAN_POINT('',(-0.6,0.,7.34788079488412E-17));
#22589=CARTESIAN_POINT('Origin',(0.,0.85,0.));
#22590=CARTESIAN_POINT('Origin',(0.,-0.9,0.));
#22591=CARTESIAN_POINT('Origin',(0.,0.,0.));
#22592=CARTESIAN_POINT('',(-1.4,0.,1.71450551880629E-16));
#22593=CARTESIAN_POINT('Origin',(0.,0.,0.));
#22594=CARTESIAN_POINT('',(1.23958209161204,0.,0.143317017690053));
#22595=CARTESIAN_POINT('',(1.22320001975977,0.,0.246749348660852));
#22596=CARTESIAN_POINT('Origin',(1.21321664662686,0.,0.192154639568406));
#22597=CARTESIAN_POINT('',(1.20190105810224,0.,0.335465908756113));
#22598=CARTESIAN_POINT('Origin',(0.,0.,0.));
#22599=CARTESIAN_POINT('',(1.16954029537568,0.,0.435062095450087));
#22600=CARTESIAN_POINT('Origin',(1.1682203282434,0.,0.379577794185952));
#22601=CARTESIAN_POINT('',(1.13462523166105,0.,0.519354515801077));
#22602=CARTESIAN_POINT('Origin',(0.,0.,0.));
#22603=CARTESIAN_POINT('',(1.08708260743774,0.,0.612662169561029));
#22604=CARTESIAN_POINT('Origin',(1.0944585482776,0.,0.557654483764164));
#22605=CARTESIAN_POINT('',(1.0394111664111,0.,0.690454891028201));
#22606=CARTESIAN_POINT('Origin',(0.,0.,0.));
#22607=CARTESIAN_POINT('',(0.977857337884349,0.,0.775176467748211));
#22608=CARTESIAN_POINT('Origin',(0.993747566553533,0.,0.72199986920298));
#22609=CARTESIAN_POINT('',(0.918603348636233,0.,0.844553975349804));
#22610=CARTESIAN_POINT('Origin',(0.,0.,0.));
#22611=CARTESIAN_POINT('',(0.844553975349804,0.,0.918603348636233));
#22612=CARTESIAN_POINT('Origin',(0.86856722168183,0.,0.86856722168183));
#22613=CARTESIAN_POINT('',(0.775176467748211,0.,0.977857337884349));
#22614=CARTESIAN_POINT('Origin',(0.,0.,0.));
#22615=CARTESIAN_POINT('',(0.690454891028201,0.,1.0394111664111));
#22616=CARTESIAN_POINT('Origin',(0.721999869202979,0.,0.993747566553533));
#22617=CARTESIAN_POINT('',(0.612662169561028,0.,1.08708260743774));
#22618=CARTESIAN_POINT('Origin',(0.,0.,0.));
#22619=CARTESIAN_POINT('',(0.519354515801077,0.,1.13462523166105));
#22620=CARTESIAN_POINT('Origin',(0.557654483764164,0.,1.0944585482776));
#22621=CARTESIAN_POINT('',(0.435062095450087,0.,1.16954029537568));
#22622=CARTESIAN_POINT('Origin',(0.,0.,0.));
#22623=CARTESIAN_POINT('',(0.335465908756113,0.,1.20190105810224));
#22624=CARTESIAN_POINT('Origin',(0.379577794185951,0.,1.1682203282434));
#22625=CARTESIAN_POINT('',(0.246749348660851,0.,1.22320001975977));
#22626=CARTESIAN_POINT('Origin',(0.,0.,0.));
#22627=CARTESIAN_POINT('',(0.143317017690053,0.,1.23958209161204));
#22628=CARTESIAN_POINT('Origin',(0.192154639568406,0.,1.21321664662686));
#22629=CARTESIAN_POINT('',(0.0523608139934478,0.,1.24674050008925));
#22630=CARTESIAN_POINT('Origin',(0.,0.,0.));
#22631=CARTESIAN_POINT('',(-0.0523608139934483,0.,1.24674050008925));
#22632=CARTESIAN_POINT('Origin',(-2.25642313758905E-16,0.,1.22833954473516));
#22633=CARTESIAN_POINT('',(-0.143317017690053,0.,1.23958209161204));
#22634=CARTESIAN_POINT('Origin',(0.,0.,0.));
#22635=CARTESIAN_POINT('',(-0.246749348660852,0.,1.22320001975977));
#22636=CARTESIAN_POINT('Origin',(-0.192154639568406,0.,1.21321664662686));
#22637=CARTESIAN_POINT('',(-0.335465908756113,0.,1.20190105810224));
#22638=CARTESIAN_POINT('Origin',(0.,0.,0.));
#22639=CARTESIAN_POINT('',(-0.435062095450087,0.,1.16954029537568));
#22640=CARTESIAN_POINT('Origin',(-0.379577794185951,0.,1.1682203282434));
#22641=CARTESIAN_POINT('',(-0.519354515801077,0.,1.13462523166105));
#22642=CARTESIAN_POINT('Origin',(0.,0.,0.));
#22643=CARTESIAN_POINT('',(-0.612662169561029,0.,1.08708260743774));
#22644=CARTESIAN_POINT('Origin',(-0.557654483764164,0.,1.0944585482776));
#22645=CARTESIAN_POINT('',(-0.690454891028201,0.,1.0394111664111));
#22646=CARTESIAN_POINT('Origin',(0.,0.,0.));
#22647=CARTESIAN_POINT('',(-0.775176467748211,0.,0.977857337884349));
#22648=CARTESIAN_POINT('Origin',(-0.721999869202979,0.,0.993747566553533));
#22649=CARTESIAN_POINT('',(-0.844553975349804,0.,0.918603348636233));
#22650=CARTESIAN_POINT('Origin',(0.,0.,0.));
#22651=CARTESIAN_POINT('',(-0.918603348636233,0.,0.844553975349804));
#22652=CARTESIAN_POINT('Origin',(-0.86856722168183,0.,0.86856722168183));
#22653=CARTESIAN_POINT('',(-0.977857337884348,0.,0.775176467748211));
#22654=CARTESIAN_POINT('Origin',(0.,0.,0.));
#22655=CARTESIAN_POINT('',(-1.0394111664111,0.,0.690454891028201));
#22656=CARTESIAN_POINT('Origin',(-0.993747566553533,0.,0.721999869202979));
#22657=CARTESIAN_POINT('',(-1.08708260743774,0.,0.612662169561028));
#22658=CARTESIAN_POINT('Origin',(0.,0.,0.));
#22659=CARTESIAN_POINT('',(-1.13462523166105,0.,0.519354515801077));
#22660=CARTESIAN_POINT('Origin',(-1.0944585482776,0.,0.557654483764164));
#22661=CARTESIAN_POINT('',(-1.16954029537568,0.,0.435062095450087));
#22662=CARTESIAN_POINT('Origin',(0.,0.,0.));
#22663=CARTESIAN_POINT('',(-1.20190105810224,0.,0.335465908756113));
#22664=CARTESIAN_POINT('Origin',(-1.1682203282434,0.,0.379577794185951));
#22665=CARTESIAN_POINT('',(-1.22320001975977,0.,0.246749348660851));
#22666=CARTESIAN_POINT('Origin',(0.,0.,0.));
#22667=CARTESIAN_POINT('',(-1.23958209161204,0.,0.143317017690053));
#22668=CARTESIAN_POINT('Origin',(-1.21321664662686,0.,0.192154639568406));
#22669=CARTESIAN_POINT('',(-1.24674050008925,0.,0.0523608139934479));
#22670=CARTESIAN_POINT('Origin',(0.,0.,0.));
#22671=CARTESIAN_POINT('',(-1.24674050008925,0.,-0.0523608139934482));
#22672=CARTESIAN_POINT('Origin',(-1.22833954473516,0.,-1.50428209172603E-16));
#22673=CARTESIAN_POINT('',(-1.23958209161204,0.,-0.143317017690053));
#22674=CARTESIAN_POINT('Origin',(0.,0.,0.));
#22675=CARTESIAN_POINT('',(-1.22320001975977,0.,-0.246749348660852));
#22676=CARTESIAN_POINT('Origin',(-1.21321664662686,0.,-0.192154639568406));
#22677=CARTESIAN_POINT('',(-1.20190105810224,0.,-0.335465908756113));
#22678=CARTESIAN_POINT('Origin',(0.,0.,0.));
#22679=CARTESIAN_POINT('',(-1.16954029537568,0.,-0.435062095450087));
#22680=CARTESIAN_POINT('Origin',(-1.1682203282434,0.,-0.379577794185951));
#22681=CARTESIAN_POINT('',(-1.13462523166105,0.,-0.519354515801077));
#22682=CARTESIAN_POINT('Origin',(0.,0.,0.));
#22683=CARTESIAN_POINT('',(-1.08708260743774,0.,-0.612662169561029));
#22684=CARTESIAN_POINT('Origin',(-1.0944585482776,0.,-0.557654483764164));
#22685=CARTESIAN_POINT('',(-1.0394111664111,0.,-0.690454891028201));
#22686=CARTESIAN_POINT('Origin',(0.,0.,0.));
#22687=CARTESIAN_POINT('',(-0.977857337884349,0.,-0.775176467748211));
#22688=CARTESIAN_POINT('Origin',(-0.993747566553533,0.,-0.721999869202979));
#22689=CARTESIAN_POINT('',(-0.918603348636233,0.,-0.844553975349804));
#22690=CARTESIAN_POINT('Origin',(0.,0.,0.));
#22691=CARTESIAN_POINT('',(-0.844553975349804,0.,-0.918603348636233));
#22692=CARTESIAN_POINT('Origin',(-0.86856722168183,0.,-0.86856722168183));
#22693=CARTESIAN_POINT('',(-0.775176467748211,0.,-0.977857337884348));
#22694=CARTESIAN_POINT('Origin',(0.,0.,0.));
#22695=CARTESIAN_POINT('',(-0.690454891028201,0.,-1.0394111664111));
#22696=CARTESIAN_POINT('Origin',(-0.721999869202979,0.,-0.993747566553533));
#22697=CARTESIAN_POINT('',(-0.612662169561028,0.,-1.08708260743774));
#22698=CARTESIAN_POINT('Origin',(0.,0.,0.));
#22699=CARTESIAN_POINT('',(-0.519354515801077,0.,-1.13462523166105));
#22700=CARTESIAN_POINT('Origin',(-0.557654483764164,0.,-1.0944585482776));
#22701=CARTESIAN_POINT('',(-0.435062095450087,0.,-1.16954029537568));
#22702=CARTESIAN_POINT('Origin',(0.,0.,0.));
#22703=CARTESIAN_POINT('',(-0.335465908756113,0.,-1.20190105810224));
#22704=CARTESIAN_POINT('Origin',(-0.379577794185951,0.,-1.1682203282434));
#22705=CARTESIAN_POINT('',(-0.246749348660852,0.,-1.22320001975977));
#22706=CARTESIAN_POINT('Origin',(0.,0.,0.));
#22707=CARTESIAN_POINT('',(-0.143317017690053,0.,-1.23958209161204));
#22708=CARTESIAN_POINT('Origin',(-0.192154639568406,0.,-1.21321664662686));
#22709=CARTESIAN_POINT('',(-0.0523608139934479,0.,-1.24674050008925));
#22710=CARTESIAN_POINT('Origin',(0.,0.,0.));
#22711=CARTESIAN_POINT('',(0.0523608139934481,0.,-1.24674050008925));
#22712=CARTESIAN_POINT('Origin',(7.52141045863017E-17,0.,-1.22833954473516));
#22713=CARTESIAN_POINT('',(0.143317017690053,0.,-1.23958209161204));
#22714=CARTESIAN_POINT('Origin',(0.,0.,0.));
#22715=CARTESIAN_POINT('',(0.246749348660852,0.,-1.22320001975977));
#22716=CARTESIAN_POINT('Origin',(0.192154639568406,0.,-1.21321664662686));
#22717=CARTESIAN_POINT('',(0.335465908756113,0.,-1.20190105810224));
#22718=CARTESIAN_POINT('Origin',(0.,0.,0.));
#22719=CARTESIAN_POINT('',(0.435062095450087,0.,-1.16954029537568));
#22720=CARTESIAN_POINT('Origin',(0.379577794185951,0.,-1.1682203282434));
#22721=CARTESIAN_POINT('',(0.519354515801077,0.,-1.13462523166105));
#22722=CARTESIAN_POINT('Origin',(0.,0.,0.));
#22723=CARTESIAN_POINT('',(0.612662169561028,0.,-1.08708260743774));
#22724=CARTESIAN_POINT('Origin',(0.557654483764164,0.,-1.0944585482776));
#22725=CARTESIAN_POINT('',(0.690454891028201,0.,-1.0394111664111));
#22726=CARTESIAN_POINT('Origin',(0.,0.,0.));
#22727=CARTESIAN_POINT('',(0.775176467748211,0.,-0.977857337884349));
#22728=CARTESIAN_POINT('Origin',(0.721999869202979,0.,-0.993747566553533));
#22729=CARTESIAN_POINT('',(0.844553975349804,0.,-0.918603348636233));
#22730=CARTESIAN_POINT('Origin',(0.,0.,0.));
#22731=CARTESIAN_POINT('',(0.918603348636233,0.,-0.844553975349804));
#22732=CARTESIAN_POINT('Origin',(0.86856722168183,0.,-0.86856722168183));
#22733=CARTESIAN_POINT('',(0.977857337884349,0.,-0.775176467748211));
#22734=CARTESIAN_POINT('Origin',(0.,0.,0.));
#22735=CARTESIAN_POINT('',(1.0394111664111,0.,-0.690454891028201));
#22736=CARTESIAN_POINT('Origin',(0.993747566553533,0.,-0.721999869202979));
#22737=CARTESIAN_POINT('',(1.08708260743774,0.,-0.612662169561028));
#22738=CARTESIAN_POINT('Origin',(0.,0.,0.));
#22739=CARTESIAN_POINT('',(1.13462523166105,0.,-0.519354515801077));
#22740=CARTESIAN_POINT('Origin',(1.0944585482776,0.,-0.557654483764164));
#22741=CARTESIAN_POINT('',(1.16954029537568,0.,-0.43506209545009));
#22742=CARTESIAN_POINT('Origin',(0.,0.,0.));
#22743=CARTESIAN_POINT('',(1.20190105810224,0.,-0.33546590875611));
#22744=CARTESIAN_POINT('Origin',(1.1682203282434,0.,-0.379577794185951));
#22745=CARTESIAN_POINT('',(1.22320001975977,0.,-0.246749348660852));
#22746=CARTESIAN_POINT('Origin',(0.,0.,0.));
#22747=CARTESIAN_POINT('',(1.23958209161204,0.,-0.143317017690053));
#22748=CARTESIAN_POINT('Origin',(1.21321664662686,0.,-0.192154639568406));
#22749=CARTESIAN_POINT('',(1.24674050008925,0.,-0.052360813993451));
#22750=CARTESIAN_POINT('Origin',(0.,0.,0.));
#22751=CARTESIAN_POINT('',(1.24674050008925,0.,0.052360813993451));
#22752=CARTESIAN_POINT('Origin',(1.22833954473516,0.,0.));
#22753=CARTESIAN_POINT('Origin',(0.,0.,0.));
#22754=CARTESIAN_POINT('Origin',(0.,0.,0.));
#22755=CARTESIAN_POINT('',(-1.4,-0.1,1.71450551880629E-16));
#22756=CARTESIAN_POINT('Origin',(0.,-0.1,0.));
#22757=CARTESIAN_POINT('',(-1.4,0.,-1.71450551880629E-16));
#22758=CARTESIAN_POINT('Origin',(0.,-0.1,0.));
#22759=CARTESIAN_POINT('Origin',(0.,0.75,0.));
#22760=CARTESIAN_POINT('',(-1.4,0.75,1.71450551880629E-16));
#22761=CARTESIAN_POINT('Origin',(0.,0.75,0.));
#22762=CARTESIAN_POINT('',(1.22320001975977,0.75,0.246749348660852));
#22763=CARTESIAN_POINT('',(1.23958209161204,0.75,0.143317017690053));
#22764=CARTESIAN_POINT('Origin',(1.21321664662686,0.75,0.192154639568406));
#22765=CARTESIAN_POINT('',(1.24674050008925,0.75,0.052360813993448));
#22766=CARTESIAN_POINT('Origin',(0.,0.75,0.));
#22767=CARTESIAN_POINT('',(1.24674050008925,0.75,-0.052360813993448));
#22768=CARTESIAN_POINT('Origin',(1.22833954473516,0.75,0.));
#22769=CARTESIAN_POINT('',(1.23958209161204,0.75,-0.143317017690053));
#22770=CARTESIAN_POINT('Origin',(0.,0.75,0.));
#22771=CARTESIAN_POINT('',(1.22320001975977,0.75,-0.246749348660852));
#22772=CARTESIAN_POINT('Origin',(1.21321664662686,0.75,-0.192154639568406));
#22773=CARTESIAN_POINT('',(1.20190105810224,0.75,-0.335465908756113));
#22774=CARTESIAN_POINT('Origin',(0.,0.75,0.));
#22775=CARTESIAN_POINT('',(1.16954029537568,0.75,-0.435062095450087));
#22776=CARTESIAN_POINT('Origin',(1.1682203282434,0.75,-0.379577794185951));
#22777=CARTESIAN_POINT('',(1.13462523166105,0.75,-0.519354515801077));
#22778=CARTESIAN_POINT('Origin',(0.,0.75,0.));
#22779=CARTESIAN_POINT('',(1.08708260743774,0.75,-0.612662169561028));
#22780=CARTESIAN_POINT('Origin',(1.0944585482776,0.75,-0.557654483764164));
#22781=CARTESIAN_POINT('',(1.0394111664111,0.75,-0.690454891028201));
#22782=CARTESIAN_POINT('Origin',(0.,0.75,0.));
#22783=CARTESIAN_POINT('',(0.977857337884349,0.75,-0.775176467748211));
#22784=CARTESIAN_POINT('Origin',(0.993747566553533,0.75,-0.721999869202979));
#22785=CARTESIAN_POINT('',(0.918603348636233,0.75,-0.844553975349804));
#22786=CARTESIAN_POINT('Origin',(0.,0.75,0.));
#22787=CARTESIAN_POINT('',(0.844553975349804,0.75,-0.918603348636233));
#22788=CARTESIAN_POINT('Origin',(0.86856722168183,0.75,-0.86856722168183));
#22789=CARTESIAN_POINT('',(0.775176467748211,0.75,-0.977857337884349));
#22790=CARTESIAN_POINT('Origin',(0.,0.75,0.));
#22791=CARTESIAN_POINT('',(0.690454891028201,0.75,-1.0394111664111));
#22792=CARTESIAN_POINT('Origin',(0.721999869202979,0.75,-0.993747566553533));
#22793=CARTESIAN_POINT('',(0.612662169561028,0.75,-1.08708260743774));
#22794=CARTESIAN_POINT('Origin',(0.,0.75,0.));
#22795=CARTESIAN_POINT('',(0.519354515801077,0.75,-1.13462523166105));
#22796=CARTESIAN_POINT('Origin',(0.557654483764164,0.75,-1.0944585482776));
#22797=CARTESIAN_POINT('',(0.435062095450087,0.75,-1.16954029537568));
#22798=CARTESIAN_POINT('Origin',(0.,0.75,0.));
#22799=CARTESIAN_POINT('',(0.335465908756113,0.75,-1.20190105810224));
#22800=CARTESIAN_POINT('Origin',(0.379577794185951,0.75,-1.1682203282434));
#22801=CARTESIAN_POINT('',(0.246749348660852,0.75,-1.22320001975977));
#22802=CARTESIAN_POINT('Origin',(0.,0.75,0.));
#22803=CARTESIAN_POINT('',(0.143317017690053,0.75,-1.23958209161204));
#22804=CARTESIAN_POINT('Origin',(0.192154639568406,0.75,-1.21321664662686));
#22805=CARTESIAN_POINT('',(0.0523608139934481,0.75,-1.24674050008925));
#22806=CARTESIAN_POINT('Origin',(0.,0.75,0.));
#22807=CARTESIAN_POINT('',(-0.0523608139934479,0.75,-1.24674050008925));
#22808=CARTESIAN_POINT('Origin',(7.52141045863017E-17,0.75,-1.22833954473516));
#22809=CARTESIAN_POINT('',(-0.143317017690053,0.75,-1.23958209161204));
#22810=CARTESIAN_POINT('Origin',(0.,0.75,0.));
#22811=CARTESIAN_POINT('',(-0.246749348660852,0.75,-1.22320001975977));
#22812=CARTESIAN_POINT('Origin',(-0.192154639568406,0.75,-1.21321664662686));
#22813=CARTESIAN_POINT('',(-0.335465908756113,0.75,-1.20190105810224));
#22814=CARTESIAN_POINT('Origin',(0.,0.75,0.));
#22815=CARTESIAN_POINT('',(-0.435062095450087,0.75,-1.16954029537568));
#22816=CARTESIAN_POINT('Origin',(-0.379577794185951,0.75,-1.1682203282434));
#22817=CARTESIAN_POINT('',(-0.519354515801077,0.75,-1.13462523166105));
#22818=CARTESIAN_POINT('Origin',(0.,0.75,0.));
#22819=CARTESIAN_POINT('',(-0.612662169561028,0.75,-1.08708260743774));
#22820=CARTESIAN_POINT('Origin',(-0.557654483764164,0.75,-1.0944585482776));
#22821=CARTESIAN_POINT('',(-0.690454891028201,0.75,-1.0394111664111));
#22822=CARTESIAN_POINT('Origin',(0.,0.75,0.));
#22823=CARTESIAN_POINT('',(-0.775176467748211,0.75,-0.977857337884348));
#22824=CARTESIAN_POINT('Origin',(-0.721999869202979,0.75,-0.993747566553533));
#22825=CARTESIAN_POINT('',(-0.844553975349804,0.75,-0.918603348636233));
#22826=CARTESIAN_POINT('Origin',(0.,0.75,0.));
#22827=CARTESIAN_POINT('',(-0.918603348636233,0.75,-0.844553975349804));
#22828=CARTESIAN_POINT('Origin',(-0.86856722168183,0.75,-0.86856722168183));
#22829=CARTESIAN_POINT('',(-0.977857337884349,0.75,-0.775176467748211));
#22830=CARTESIAN_POINT('Origin',(0.,0.75,0.));
#22831=CARTESIAN_POINT('',(-1.0394111664111,0.75,-0.690454891028201));
#22832=CARTESIAN_POINT('Origin',(-0.993747566553533,0.75,-0.721999869202979));
#22833=CARTESIAN_POINT('',(-1.08708260743774,0.75,-0.612662169561029));
#22834=CARTESIAN_POINT('Origin',(0.,0.75,0.));
#22835=CARTESIAN_POINT('',(-1.13462523166105,0.75,-0.519354515801077));
#22836=CARTESIAN_POINT('Origin',(-1.0944585482776,0.75,-0.557654483764164));
#22837=CARTESIAN_POINT('',(-1.16954029537568,0.75,-0.435062095450087));
#22838=CARTESIAN_POINT('Origin',(0.,0.75,0.));
#22839=CARTESIAN_POINT('',(-1.20190105810224,0.75,-0.335465908756113));
#22840=CARTESIAN_POINT('Origin',(-1.1682203282434,0.75,-0.379577794185951));
#22841=CARTESIAN_POINT('',(-1.22320001975977,0.75,-0.246749348660852));
#22842=CARTESIAN_POINT('Origin',(0.,0.75,0.));
#22843=CARTESIAN_POINT('',(-1.23958209161204,0.75,-0.143317017690053));
#22844=CARTESIAN_POINT('Origin',(-1.21321664662686,0.75,-0.192154639568406));
#22845=CARTESIAN_POINT('',(-1.24674050008925,0.75,-0.0523608139934482));
#22846=CARTESIAN_POINT('Origin',(0.,0.75,0.));
#22847=CARTESIAN_POINT('',(-1.24674050008925,0.75,0.0523608139934479));
#22848=CARTESIAN_POINT('Origin',(-1.22833954473516,0.75,-1.50428209172603E-16));
#22849=CARTESIAN_POINT('',(-1.23958209161204,0.75,0.143317017690053));
#22850=CARTESIAN_POINT('Origin',(0.,0.75,0.));
#22851=CARTESIAN_POINT('',(-1.22320001975977,0.75,0.246749348660851));
#22852=CARTESIAN_POINT('Origin',(-1.21321664662686,0.75,0.192154639568406));
#22853=CARTESIAN_POINT('',(-1.20190105810224,0.75,0.335465908756113));
#22854=CARTESIAN_POINT('Origin',(0.,0.75,0.));
#22855=CARTESIAN_POINT('',(-1.16954029537568,0.75,0.435062095450087));
#22856=CARTESIAN_POINT('Origin',(-1.1682203282434,0.75,0.379577794185951));
#22857=CARTESIAN_POINT('',(-1.13462523166105,0.75,0.519354515801077));
#22858=CARTESIAN_POINT('Origin',(0.,0.75,0.));
#22859=CARTESIAN_POINT('',(-1.08708260743774,0.75,0.612662169561028));
#22860=CARTESIAN_POINT('Origin',(-1.0944585482776,0.75,0.557654483764164));
#22861=CARTESIAN_POINT('',(-1.0394111664111,0.75,0.690454891028201));
#22862=CARTESIAN_POINT('Origin',(0.,0.75,0.));
#22863=CARTESIAN_POINT('',(-0.977857337884348,0.75,0.775176467748211));
#22864=CARTESIAN_POINT('Origin',(-0.993747566553533,0.75,0.721999869202979));
#22865=CARTESIAN_POINT('',(-0.918603348636233,0.75,0.844553975349804));
#22866=CARTESIAN_POINT('Origin',(0.,0.75,0.));
#22867=CARTESIAN_POINT('',(-0.844553975349804,0.75,0.918603348636233));
#22868=CARTESIAN_POINT('Origin',(-0.86856722168183,0.75,0.86856722168183));
#22869=CARTESIAN_POINT('',(-0.775176467748211,0.75,0.977857337884349));
#22870=CARTESIAN_POINT('Origin',(0.,0.75,0.));
#22871=CARTESIAN_POINT('',(-0.690454891028201,0.75,1.0394111664111));
#22872=CARTESIAN_POINT('Origin',(-0.721999869202979,0.75,0.993747566553533));
#22873=CARTESIAN_POINT('',(-0.612662169561029,0.75,1.08708260743774));
#22874=CARTESIAN_POINT('Origin',(0.,0.75,0.));
#22875=CARTESIAN_POINT('',(-0.519354515801077,0.75,1.13462523166105));
#22876=CARTESIAN_POINT('Origin',(-0.557654483764164,0.75,1.0944585482776));
#22877=CARTESIAN_POINT('',(-0.435062095450087,0.75,1.16954029537568));
#22878=CARTESIAN_POINT('Origin',(0.,0.75,0.));
#22879=CARTESIAN_POINT('',(-0.335465908756113,0.75,1.20190105810224));
#22880=CARTESIAN_POINT('Origin',(-0.379577794185951,0.75,1.1682203282434));
#22881=CARTESIAN_POINT('',(-0.246749348660852,0.75,1.22320001975977));
#22882=CARTESIAN_POINT('Origin',(0.,0.75,0.));
#22883=CARTESIAN_POINT('',(-0.143317017690053,0.75,1.23958209161204));
#22884=CARTESIAN_POINT('Origin',(-0.192154639568406,0.75,1.21321664662686));
#22885=CARTESIAN_POINT('',(-0.0523608139934483,0.75,1.24674050008925));
#22886=CARTESIAN_POINT('Origin',(0.,0.75,0.));
#22887=CARTESIAN_POINT('',(0.0523608139934478,0.75,1.24674050008925));
#22888=CARTESIAN_POINT('Origin',(-2.25642313758905E-16,0.75,1.22833954473516));
#22889=CARTESIAN_POINT('',(0.143317017690053,0.75,1.23958209161204));
#22890=CARTESIAN_POINT('Origin',(0.,0.75,0.));
#22891=CARTESIAN_POINT('',(0.246749348660851,0.75,1.22320001975977));
#22892=CARTESIAN_POINT('Origin',(0.192154639568406,0.75,1.21321664662686));
#22893=CARTESIAN_POINT('',(0.335465908756113,0.75,1.20190105810224));
#22894=CARTESIAN_POINT('Origin',(0.,0.75,0.));
#22895=CARTESIAN_POINT('',(0.435062095450087,0.75,1.16954029537568));
#22896=CARTESIAN_POINT('Origin',(0.379577794185951,0.75,1.1682203282434));
#22897=CARTESIAN_POINT('',(0.519354515801077,0.75,1.13462523166105));
#22898=CARTESIAN_POINT('Origin',(0.,0.75,0.));
#22899=CARTESIAN_POINT('',(0.612662169561028,0.75,1.08708260743774));
#22900=CARTESIAN_POINT('Origin',(0.557654483764164,0.75,1.0944585482776));
#22901=CARTESIAN_POINT('',(0.690454891028201,0.75,1.0394111664111));
#22902=CARTESIAN_POINT('Origin',(0.,0.75,0.));
#22903=CARTESIAN_POINT('',(0.775176467748211,0.75,0.977857337884349));
#22904=CARTESIAN_POINT('Origin',(0.721999869202979,0.75,0.993747566553533));
#22905=CARTESIAN_POINT('',(0.844553975349804,0.75,0.918603348636233));
#22906=CARTESIAN_POINT('Origin',(0.,0.75,0.));
#22907=CARTESIAN_POINT('',(0.918603348636233,0.75,0.844553975349804));
#22908=CARTESIAN_POINT('Origin',(0.86856722168183,0.75,0.86856722168183));
#22909=CARTESIAN_POINT('',(0.977857337884349,0.75,0.775176467748211));
#22910=CARTESIAN_POINT('Origin',(0.,0.75,0.));
#22911=CARTESIAN_POINT('',(1.0394111664111,0.75,0.690454891028201));
#22912=CARTESIAN_POINT('Origin',(0.993747566553533,0.75,0.72199986920298));
#22913=CARTESIAN_POINT('',(1.08708260743774,0.75,0.612662169561029));
#22914=CARTESIAN_POINT('Origin',(0.,0.75,0.));
#22915=CARTESIAN_POINT('',(1.13462523166105,0.75,0.519354515801077));
#22916=CARTESIAN_POINT('Origin',(1.0944585482776,0.75,0.557654483764164));
#22917=CARTESIAN_POINT('',(1.16954029537568,0.75,0.435062095450087));
#22918=CARTESIAN_POINT('Origin',(0.,0.75,0.));
#22919=CARTESIAN_POINT('',(1.20190105810224,0.75,0.335465908756113));
#22920=CARTESIAN_POINT('Origin',(1.1682203282434,0.75,0.379577794185952));
#22921=CARTESIAN_POINT('Origin',(0.,0.75,0.));
#22922=CARTESIAN_POINT('Origin',(0.,0.75,0.));
#22923=CARTESIAN_POINT('',(-1.4,0.85,1.71450551880629E-16));
#22924=CARTESIAN_POINT('Origin',(0.,0.85,0.));
#22925=CARTESIAN_POINT('',(-1.4,0.75,1.71450551880629E-16));
#22926=CARTESIAN_POINT('Origin',(0.,0.85,0.));
#22927=CARTESIAN_POINT('Origin',(1.21321664662686,0.,0.192154639568406));
#22928=CARTESIAN_POINT('',(1.23958209161204,0.,0.14331701769005));
#22929=CARTESIAN_POINT('',(1.22320001975977,0.,0.246749348660855));
#22930=CARTESIAN_POINT('Origin',(0.,0.,0.));
#22931=CARTESIAN_POINT('',(1.20190105810224,0.,0.33546590875611));
#22932=CARTESIAN_POINT('Origin',(1.1682203282434,0.,0.379577794185952));
#22933=CARTESIAN_POINT('',(1.16954029537568,0.,0.43506209545009));
#22934=CARTESIAN_POINT('Origin',(0.,0.,0.));
#22935=CARTESIAN_POINT('',(1.13462523166105,0.,0.519354515801074));
#22936=CARTESIAN_POINT('Origin',(1.0944585482776,0.,0.557654483764164));
#22937=CARTESIAN_POINT('',(1.08708260743774,0.,0.612662169561031));
#22938=CARTESIAN_POINT('Origin',(0.,0.,0.));
#22939=CARTESIAN_POINT('',(1.03941116641111,0.,0.690454891028199));
#22940=CARTESIAN_POINT('Origin',(0.993747566553533,0.,0.72199986920298));
#22941=CARTESIAN_POINT('',(0.977857337884347,0.,0.775176467748214));
#22942=CARTESIAN_POINT('Origin',(0.,0.,0.));
#22943=CARTESIAN_POINT('',(0.918603348636235,0.,0.844553975349802));
#22944=CARTESIAN_POINT('Origin',(0.86856722168183,0.,0.86856722168183));
#22945=CARTESIAN_POINT('',(0.844553975349802,0.,0.918603348636235));
#22946=CARTESIAN_POINT('Origin',(0.,0.,0.));
#22947=CARTESIAN_POINT('',(0.775176467748213,0.,0.977857337884347));
#22948=CARTESIAN_POINT('Origin',(0.721999869202979,0.,0.993747566553533));
#22949=CARTESIAN_POINT('',(0.690454891028198,0.,1.03941116641111));
#22950=CARTESIAN_POINT('Origin',(0.,0.,0.));
#22951=CARTESIAN_POINT('',(0.612662169561031,0.,1.08708260743774));
#22952=CARTESIAN_POINT('Origin',(0.557654483764164,0.,1.0944585482776));
#22953=CARTESIAN_POINT('',(0.519354515801074,0.,1.13462523166105));
#22954=CARTESIAN_POINT('Origin',(0.,0.,0.));
#22955=CARTESIAN_POINT('',(0.43506209545009,0.,1.16954029537568));
#22956=CARTESIAN_POINT('Origin',(0.379577794185951,0.,1.1682203282434));
#22957=CARTESIAN_POINT('',(0.33546590875611,0.,1.20190105810224));
#22958=CARTESIAN_POINT('Origin',(0.,0.,0.));
#22959=CARTESIAN_POINT('',(0.246749348660854,0.,1.22320001975977));
#22960=CARTESIAN_POINT('Origin',(0.192154639568406,0.,1.21321664662686));
#22961=CARTESIAN_POINT('',(0.14331701769005,0.,1.23958209161204));
#22962=CARTESIAN_POINT('Origin',(0.,0.,0.));
#22963=CARTESIAN_POINT('',(0.0523608139934508,0.,1.24674050008925));
#22964=CARTESIAN_POINT('Origin',(-2.25642313758905E-16,0.,1.22833954473516));
#22965=CARTESIAN_POINT('',(-0.0523608139934513,0.,1.24674050008925));
#22966=CARTESIAN_POINT('Origin',(0.,0.,0.));
#22967=CARTESIAN_POINT('',(-0.14331701769005,0.,1.23958209161204));
#22968=CARTESIAN_POINT('Origin',(-0.192154639568406,0.,1.21321664662686));
#22969=CARTESIAN_POINT('',(-0.246749348660855,0.,1.22320001975977));
#22970=CARTESIAN_POINT('Origin',(0.,0.,0.));
#22971=CARTESIAN_POINT('',(-0.33546590875611,0.,1.20190105810224));
#22972=CARTESIAN_POINT('Origin',(-0.379577794185951,0.,1.1682203282434));
#22973=CARTESIAN_POINT('',(-0.43506209545009,0.,1.16954029537568));
#22974=CARTESIAN_POINT('Origin',(0.,0.,0.));
#22975=CARTESIAN_POINT('',(-0.519354515801074,0.,1.13462523166105));
#22976=CARTESIAN_POINT('Origin',(-0.557654483764164,0.,1.0944585482776));
#22977=CARTESIAN_POINT('',(-0.612662169561031,0.,1.08708260743774));
#22978=CARTESIAN_POINT('Origin',(0.,0.,0.));
#22979=CARTESIAN_POINT('',(-0.690454891028199,0.,1.03941116641111));
#22980=CARTESIAN_POINT('Origin',(-0.721999869202979,0.,0.993747566553533));
#22981=CARTESIAN_POINT('',(-0.775176467748213,0.,0.977857337884347));
#22982=CARTESIAN_POINT('Origin',(0.,0.,0.));
#22983=CARTESIAN_POINT('',(-0.844553975349802,0.,0.918603348636235));
#22984=CARTESIAN_POINT('Origin',(-0.86856722168183,0.,0.86856722168183));
#22985=CARTESIAN_POINT('',(-0.918603348636235,0.,0.844553975349802));
#22986=CARTESIAN_POINT('Origin',(0.,0.,0.));
#22987=CARTESIAN_POINT('',(-0.977857337884347,0.,0.775176467748213));
#22988=CARTESIAN_POINT('Origin',(-0.993747566553533,0.,0.721999869202979));
#22989=CARTESIAN_POINT('',(-1.03941116641111,0.,0.690454891028198));
#22990=CARTESIAN_POINT('Origin',(0.,0.,0.));
#22991=CARTESIAN_POINT('',(-1.08708260743774,0.,0.612662169561031));
#22992=CARTESIAN_POINT('Origin',(-1.0944585482776,0.,0.557654483764164));
#22993=CARTESIAN_POINT('',(-1.13462523166105,0.,0.519354515801074));
#22994=CARTESIAN_POINT('Origin',(0.,0.,0.));
#22995=CARTESIAN_POINT('',(-1.16954029537568,0.,0.43506209545009));
#22996=CARTESIAN_POINT('Origin',(-1.1682203282434,0.,0.379577794185951));
#22997=CARTESIAN_POINT('',(-1.20190105810224,0.,0.33546590875611));
#22998=CARTESIAN_POINT('Origin',(0.,0.,0.));
#22999=CARTESIAN_POINT('',(-1.22320001975977,0.,0.246749348660854));
#23000=CARTESIAN_POINT('Origin',(-1.21321664662686,0.,0.192154639568406));
#23001=CARTESIAN_POINT('',(-1.23958209161204,0.,0.14331701769005));
#23002=CARTESIAN_POINT('Origin',(0.,0.,0.));
#23003=CARTESIAN_POINT('',(-1.24674050008925,0.,0.0523608139934509));
#23004=CARTESIAN_POINT('Origin',(-1.22833954473516,0.,-1.50428209172603E-16));
#23005=CARTESIAN_POINT('',(-1.24674050008925,0.,-0.0523608139934512));
#23006=CARTESIAN_POINT('Origin',(0.,0.,0.));
#23007=CARTESIAN_POINT('',(-1.23958209161204,0.,-0.14331701769005));
#23008=CARTESIAN_POINT('Origin',(-1.21321664662686,0.,-0.192154639568406));
#23009=CARTESIAN_POINT('',(-1.22320001975977,0.,-0.246749348660855));
#23010=CARTESIAN_POINT('Origin',(0.,0.,0.));
#23011=CARTESIAN_POINT('',(-1.20190105810224,0.,-0.33546590875611));
#23012=CARTESIAN_POINT('Origin',(-1.1682203282434,0.,-0.379577794185951));
#23013=CARTESIAN_POINT('',(-1.16954029537568,0.,-0.43506209545009));
#23014=CARTESIAN_POINT('Origin',(0.,0.,0.));
#23015=CARTESIAN_POINT('',(-1.13462523166105,0.,-0.519354515801074));
#23016=CARTESIAN_POINT('Origin',(-1.0944585482776,0.,-0.557654483764164));
#23017=CARTESIAN_POINT('',(-1.08708260743774,0.,-0.612662169561031));
#23018=CARTESIAN_POINT('Origin',(0.,0.,0.));
#23019=CARTESIAN_POINT('',(-1.03941116641111,0.,-0.690454891028199));
#23020=CARTESIAN_POINT('Origin',(-0.993747566553533,0.,-0.721999869202979));
#23021=CARTESIAN_POINT('',(-0.977857337884347,0.,-0.775176467748213));
#23022=CARTESIAN_POINT('Origin',(0.,0.,0.));
#23023=CARTESIAN_POINT('',(-0.918603348636235,0.,-0.844553975349802));
#23024=CARTESIAN_POINT('Origin',(-0.86856722168183,0.,-0.86856722168183));
#23025=CARTESIAN_POINT('',(-0.844553975349802,0.,-0.918603348636235));
#23026=CARTESIAN_POINT('Origin',(0.,0.,0.));
#23027=CARTESIAN_POINT('',(-0.775176467748213,0.,-0.977857337884347));
#23028=CARTESIAN_POINT('Origin',(-0.721999869202979,0.,-0.993747566553533));
#23029=CARTESIAN_POINT('',(-0.690454891028198,0.,-1.03941116641111));
#23030=CARTESIAN_POINT('Origin',(0.,0.,0.));
#23031=CARTESIAN_POINT('',(-0.612662169561031,0.,-1.08708260743774));
#23032=CARTESIAN_POINT('Origin',(-0.557654483764164,0.,-1.0944585482776));
#23033=CARTESIAN_POINT('',(-0.519354515801074,0.,-1.13462523166105));
#23034=CARTESIAN_POINT('Origin',(0.,0.,0.));
#23035=CARTESIAN_POINT('',(-0.43506209545009,0.,-1.16954029537568));
#23036=CARTESIAN_POINT('Origin',(-0.379577794185951,0.,-1.1682203282434));
#23037=CARTESIAN_POINT('',(-0.33546590875611,0.,-1.20190105810224));
#23038=CARTESIAN_POINT('Origin',(0.,0.,0.));
#23039=CARTESIAN_POINT('',(-0.246749348660854,0.,-1.22320001975977));
#23040=CARTESIAN_POINT('Origin',(-0.192154639568406,0.,-1.21321664662686));
#23041=CARTESIAN_POINT('',(-0.14331701769005,0.,-1.23958209161204));
#23042=CARTESIAN_POINT('Origin',(0.,0.,0.));
#23043=CARTESIAN_POINT('',(-0.052360813993451,0.,-1.24674050008925));
#23044=CARTESIAN_POINT('Origin',(7.52141045863017E-17,0.,-1.22833954473516));
#23045=CARTESIAN_POINT('',(0.0523608139934511,0.,-1.24674050008925));
#23046=CARTESIAN_POINT('Origin',(0.,0.,0.));
#23047=CARTESIAN_POINT('',(0.14331701769005,0.,-1.23958209161204));
#23048=CARTESIAN_POINT('Origin',(0.192154639568406,0.,-1.21321664662686));
#23049=CARTESIAN_POINT('',(0.246749348660855,0.,-1.22320001975977));
#23050=CARTESIAN_POINT('Origin',(0.,0.,0.));
#23051=CARTESIAN_POINT('',(0.33546590875611,0.,-1.20190105810224));
#23052=CARTESIAN_POINT('Origin',(0.379577794185951,0.,-1.1682203282434));
#23053=CARTESIAN_POINT('',(0.43506209545009,0.,-1.16954029537568));
#23054=CARTESIAN_POINT('Origin',(0.,0.,0.));
#23055=CARTESIAN_POINT('',(0.519354515801074,0.,-1.13462523166105));
#23056=CARTESIAN_POINT('Origin',(0.557654483764164,0.,-1.0944585482776));
#23057=CARTESIAN_POINT('',(0.612662169561031,0.,-1.08708260743774));
#23058=CARTESIAN_POINT('Origin',(0.,0.,0.));
#23059=CARTESIAN_POINT('',(0.690454891028198,0.,-1.03941116641111));
#23060=CARTESIAN_POINT('Origin',(0.721999869202979,0.,-0.993747566553533));
#23061=CARTESIAN_POINT('',(0.775176467748213,0.,-0.977857337884347));
#23062=CARTESIAN_POINT('Origin',(0.,0.,0.));
#23063=CARTESIAN_POINT('',(0.844553975349802,0.,-0.918603348636235));
#23064=CARTESIAN_POINT('Origin',(0.86856722168183,0.,-0.86856722168183));
#23065=CARTESIAN_POINT('',(0.918603348636235,0.,-0.844553975349802));
#23066=CARTESIAN_POINT('Origin',(0.,0.,0.));
#23067=CARTESIAN_POINT('',(0.977857337884347,0.,-0.775176467748213));
#23068=CARTESIAN_POINT('Origin',(0.993747566553533,0.,-0.721999869202979));
#23069=CARTESIAN_POINT('',(1.03941116641111,0.,-0.690454891028198));
#23070=CARTESIAN_POINT('Origin',(0.,0.,0.));
#23071=CARTESIAN_POINT('',(1.08708260743774,0.,-0.612662169561031));
#23072=CARTESIAN_POINT('Origin',(1.0944585482776,0.,-0.557654483764164));
#23073=CARTESIAN_POINT('',(1.13462523166105,0.,-0.519354515801074));
#23074=CARTESIAN_POINT('Origin',(0.,0.,0.));
#23075=CARTESIAN_POINT('',(1.16954029537568,0.,-0.43506209545009));
#23076=CARTESIAN_POINT('Origin',(1.1682203282434,0.,-0.379577794185951));
#23077=CARTESIAN_POINT('',(1.20190105810224,0.,-0.33546590875611));
#23078=CARTESIAN_POINT('Origin',(0.,0.,0.));
#23079=CARTESIAN_POINT('',(1.22320001975977,0.,-0.246749348660855));
#23080=CARTESIAN_POINT('Origin',(1.21321664662686,0.,-0.192154639568406));
#23081=CARTESIAN_POINT('',(1.23958209161204,0.,-0.14331701769005));
#23082=CARTESIAN_POINT('Origin',(0.,0.,0.));
#23083=CARTESIAN_POINT('',(1.24674050008925,0.,0.052360813993451));
#23084=CARTESIAN_POINT('Origin',(1.22833954473516,0.,0.));
#23085=CARTESIAN_POINT('',(1.24674050008925,0.,-0.052360813993451));
#23086=CARTESIAN_POINT('Origin',(0.,0.,0.));
#23087=CARTESIAN_POINT('',(0.,0.,0.));
#23088=CARTESIAN_POINT('Origin',(0.3,0.4,0.));
#23089=CARTESIAN_POINT('',(-0.3,0.4,-3.67394039744206E-17));
#23090=CARTESIAN_POINT('Origin',(0.,0.4,0.));
#23091=CARTESIAN_POINT('Origin',(0.,0.375,0.));
#23092=CARTESIAN_POINT('',(-0.35,0.35,-4.28626379701573E-17));
#23093=CARTESIAN_POINT('Origin',(0.,0.35,0.));
#23094=CARTESIAN_POINT('',(-0.325,0.375,-3.9801020972289E-17));
#23095=CARTESIAN_POINT('Origin',(0.,0.19,0.));
#23096=CARTESIAN_POINT('',(-0.35,0.03,-4.28626379701574E-17));
#23097=CARTESIAN_POINT('Origin',(0.,0.03,0.));
#23098=CARTESIAN_POINT('',(-0.35,0.19,-4.28626379701574E-17));
#23099=CARTESIAN_POINT('Origin',(0.,0.0149999999999999,0.));
#23100=CARTESIAN_POINT('',(-0.32,-3.29597460435593E-17,-3.91886975727153E-17));
#23101=CARTESIAN_POINT('Origin',(0.,0.,0.));
#23102=CARTESIAN_POINT('',(-0.335,0.0149999999999999,-4.10256677714363E-17));
#23103=CARTESIAN_POINT('Origin',(0.22,0.,0.));
#23104=CARTESIAN_POINT('',(-0.22,-6.93889390390723E-18,-2.69422295812418E-17));
#23105=CARTESIAN_POINT('Origin',(0.,0.,0.));
#23106=CARTESIAN_POINT('Origin',(0.,-0.02,0.));
#23107=CARTESIAN_POINT('',(-0.1954,-0.0492,2.39295984553393E-17));
#23108=CARTESIAN_POINT('Origin',(0.,-0.0492,0.));
#23109=CARTESIAN_POINT('',(-0.21,-0.02,-2.57175827820944E-17));
#23110=CARTESIAN_POINT('Origin',(0.,-0.8,0.));
#23111=CARTESIAN_POINT('',(-0.1954,-1.5646,2.39295984553393E-17));
#23112=CARTESIAN_POINT('Origin',(0.,-1.5646,0.));
#23113=CARTESIAN_POINT('',(-0.1954,-0.8,-2.39295984553393E-17));
#23114=CARTESIAN_POINT('Origin',(0.,-1.58,0.));
#23115=CARTESIAN_POINT('',(-0.16,-1.6,-1.95943487863577E-17));
#23116=CARTESIAN_POINT('Origin',(0.,-1.6,0.));
#23117=CARTESIAN_POINT('',(-0.18,-1.58,-2.20436423846524E-17));
#23118=CARTESIAN_POINT('Origin',(0.,-1.6,0.));
#23119=CARTESIAN_POINT('Origin',(0.0866025403784439,-0.4,-0.15));
#23120=CARTESIAN_POINT('',(0.173205080756888,-0.4,0.));
#23121=CARTESIAN_POINT('',(0.0866025403784439,-0.4,-0.15));
#23122=CARTESIAN_POINT('',(0.173205080756888,-0.4,0.));
#23123=CARTESIAN_POINT('',(0.0866025403784439,-0.64,-0.15));
#23124=CARTESIAN_POINT('',(0.0866025403784439,-0.4,-0.15));
#23125=CARTESIAN_POINT('',(0.173205080756888,-0.64,0.));
#23126=CARTESIAN_POINT('',(0.173205080756888,-0.64,0.));
#23127=CARTESIAN_POINT('',(0.173205080756888,-0.4,0.));
#23128=CARTESIAN_POINT('Origin',(-0.0866025403784438,-0.4,-0.15));
#23129=CARTESIAN_POINT('',(-0.0866025403784438,-0.4,-0.15));
#23130=CARTESIAN_POINT('',(0.0866025403784439,-0.4,-0.15));
#23131=CARTESIAN_POINT('',(-0.0866025403784438,-0.64,-0.15));
#23132=CARTESIAN_POINT('',(-0.0866025403784438,-0.4,-0.15));
#23133=CARTESIAN_POINT('',(0.0866025403784439,-0.64,-0.15));
#23134=CARTESIAN_POINT('Origin',(-0.173205080756888,-0.4,-2.77555756156289E-17));
#23135=CARTESIAN_POINT('',(-0.173205080756888,-0.4,-2.12115047744981E-17));
#23136=CARTESIAN_POINT('',(-0.0866025403784438,-0.4,-0.15));
#23137=CARTESIAN_POINT('',(-0.173205080756888,-0.64,-2.77555756156289E-17));
#23138=CARTESIAN_POINT('',(-0.173205080756888,-0.4,-2.12115047744981E-17));
#23139=CARTESIAN_POINT('',(-0.0866025403784438,-0.64,-0.15));
#23140=CARTESIAN_POINT('Origin',(-0.0866025403784439,-0.4,0.15));
#23141=CARTESIAN_POINT('',(-0.0866025403784439,-0.4,0.15));
#23142=CARTESIAN_POINT('',(-0.173205080756888,-0.4,-2.12115047744981E-17));
#23143=CARTESIAN_POINT('',(-0.0866025403784439,-0.64,0.15));
#23144=CARTESIAN_POINT('',(-0.0866025403784439,-0.4,0.15));
#23145=CARTESIAN_POINT('',(-0.173205080756888,-0.64,-2.12115047744981E-17));
#23146=CARTESIAN_POINT('Origin',(0.0866025403784439,-0.4,0.15));
#23147=CARTESIAN_POINT('',(0.0866025403784439,-0.4,0.15));
#23148=CARTESIAN_POINT('',(-0.0866025403784439,-0.4,0.15));
#23149=CARTESIAN_POINT('',(0.0866025403784439,-0.64,0.15));
#23150=CARTESIAN_POINT('',(0.0866025403784439,-0.4,0.15));
#23151=CARTESIAN_POINT('',(-0.0866025403784439,-0.64,0.15));
#23152=CARTESIAN_POINT('Origin',(0.173205080756888,-0.4,0.));
#23153=CARTESIAN_POINT('',(0.0866025403784439,-0.4,0.15));
#23154=CARTESIAN_POINT('',(0.0866025403784439,-0.64,0.15));
#23155=CARTESIAN_POINT('Origin',(0.,-0.4,-2.77555756156289E-17));
#23156=CARTESIAN_POINT('Origin',(0.,-0.64,-2.77555756156289E-17));
#23157=CARTESIAN_POINT('',(0.,0.,0.));
#23158=CARTESIAN_POINT('',(0.,0.,0.));
#23159=CARTESIAN_POINT('',(0.,0.,0.));
#23160=CARTESIAN_POINT('',(0.,0.,0.));
#23161=CARTESIAN_POINT('',(0.,0.,0.));
#23162=CARTESIAN_POINT('',(0.,0.,0.));
#23163=CARTESIAN_POINT('',(0.,0.,0.));
#23164=CARTESIAN_POINT('',(0.,0.,0.));
#23165=CARTESIAN_POINT('',(0.,0.,0.));
#23166=CARTESIAN_POINT('',(0.,0.,0.));
#23167=CARTESIAN_POINT('',(0.,0.,0.));
#23168=CARTESIAN_POINT('',(0.,0.,0.));
#23169=CARTESIAN_POINT('',(0.,0.,0.));
#23170=CARTESIAN_POINT('',(4.,0.,0.));
#23171=CARTESIAN_POINT('',(6.,0.,0.97));
#23172=CARTESIAN_POINT('',(12.,0.,0.97));
#23173=CARTESIAN_POINT('',(18.,0.,0.97));
#23174=CARTESIAN_POINT('',(24.,0.,0.97));
#23175=CARTESIAN_POINT('',(-2.8,-1.,0.8));
#23176=CARTESIAN_POINT('',(-2.8,1.,0.8));
#23177=CARTESIAN_POINT('',(2.8,-1.,0.8));
#23178=CARTESIAN_POINT('',(2.8,1.,0.8));
#23179=CARTESIAN_POINT('',(0.,-0.9,7.));
#23180=CARTESIAN_POINT('',(0.,0.9,7.));
#23181=CARTESIAN_POINT('',(1.34350288425444,-2.1,8.34350288425444));
#23182=CARTESIAN_POINT('',(-1.34350288425444,-2.1,8.34350288425444));
#23183=CARTESIAN_POINT('',(-1.34350288425444,-2.1,5.65649711574556));
#23184=CARTESIAN_POINT('',(1.34350288425444,-2.1,5.65649711574556));
#23185=CARTESIAN_POINT('',(1.34350288425444,2.1,8.34350288425444));
#23186=CARTESIAN_POINT('',(-1.34350288425444,2.1,8.34350288425444));
#23187=CARTESIAN_POINT('',(-1.34350288425444,2.1,5.65649711574556));
#23188=CARTESIAN_POINT('',(1.34350288425444,2.1,5.65649711574556));
#23189=CARTESIAN_POINT('',(2.75,9.5,0.6));
#23190=CARTESIAN_POINT('',(2.75,12.5,0.6));
#23191=CARTESIAN_POINT('',(22.25,9.5,0.6));
#23192=CARTESIAN_POINT('',(22.25,12.5,0.6));
#23193=CARTESIAN_POINT('',(3.,6.9,0.6));
#23194=CARTESIAN_POINT('',(3.,8.1,0.6));
#23195=CARTESIAN_POINT('',(0.,0.,0.));
#23196=CARTESIAN_POINT('',(0.,0.,0.));
#23197=CARTESIAN_POINT('',(0.,0.,0.));
#23198=CARTESIAN_POINT('',(0.,0.,0.));
#23199=CARTESIAN_POINT('',(0.,0.,0.));
#23200=CARTESIAN_POINT('',(0.,0.,0.));
#23201=CARTESIAN_POINT('',(0.,-3.5,7.));
#23202=CARTESIAN_POINT('',(0.,-5.2,7.));
#23203=CARTESIAN_POINT('',(0.,0.,0.));
#23204=CARTESIAN_POINT('',(0.,0.,0.));
#23205=CARTESIAN_POINT('',(0.,0.,0.));
#23206=CARTESIAN_POINT('',(0.,0.,0.));
#23207=CARTESIAN_POINT('',(0.,0.,0.));
#23208=CARTESIAN_POINT('',(0.,0.,0.));
#23209=CARTESIAN_POINT('',(10.,-3.5,7.));
#23210=CARTESIAN_POINT('',(10.,-5.2,7.));
#23211=CARTESIAN_POINT('',(0.,0.,0.));
#23212=CARTESIAN_POINT('',(0.,0.,0.));
#23213=CARTESIAN_POINT('Origin',(-0.2,11.,4.5));
#23214=CARTESIAN_POINT('',(1.,11.,4.9));
#23215=CARTESIAN_POINT('Origin',(1.,11.,4.5));
#23216=CARTESIAN_POINT('',(-0.2,11.,4.9));
#23217=CARTESIAN_POINT('',(-0.2,11.,4.9));
#23218=CARTESIAN_POINT('Origin',(-0.2,11.,4.5));
#23219=CARTESIAN_POINT('Origin',(-0.2,11.,4.5));
#23220=CARTESIAN_POINT('Origin',(23.4,11.,4.5));
#23221=CARTESIAN_POINT('',(23.4,11.,5.4));
#23222=CARTESIAN_POINT('Origin',(23.4,11.,4.5));
#23223=CARTESIAN_POINT('',(23.4,11.,5.1));
#23224=CARTESIAN_POINT('Origin',(23.4,11.,4.5));
#23225=CARTESIAN_POINT('Origin',(23.,11.,4.5));
#23226=CARTESIAN_POINT('',(23.,11.,5.4));
#23227=CARTESIAN_POINT('Origin',(23.,11.,4.5));
#23228=CARTESIAN_POINT('',(23.,11.,5.1));
#23229=CARTESIAN_POINT('Origin',(23.,11.,4.5));
#23230=CARTESIAN_POINT('Origin',(23.,11.,4.5));
#23231=CARTESIAN_POINT('',(23.,11.,5.4));
#23232=CARTESIAN_POINT('Origin',(21.5,11.,4.5));
#23233=CARTESIAN_POINT('',(21.5,11.,5.1));
#23234=CARTESIAN_POINT('',(21.5,11.,5.1));
#23235=CARTESIAN_POINT('Origin',(21.5,11.,4.5));
#23236=CARTESIAN_POINT('Origin',(2.,11.,4.5));
#23237=CARTESIAN_POINT('',(2.,11.,5.4));
#23238=CARTESIAN_POINT('Origin',(2.,11.,4.5));
#23239=CARTESIAN_POINT('',(2.,11.,5.1));
#23240=CARTESIAN_POINT('Origin',(2.,11.,4.5));
#23241=CARTESIAN_POINT('Origin',(1.6,11.,4.5));
#23242=CARTESIAN_POINT('',(1.6,11.,5.4));
#23243=CARTESIAN_POINT('Origin',(1.6,11.,4.5));
#23244=CARTESIAN_POINT('',(1.6,11.,5.1));
#23245=CARTESIAN_POINT('Origin',(1.6,11.,4.5));
#23246=CARTESIAN_POINT('Origin',(1.6,11.,4.5));
#23247=CARTESIAN_POINT('',(1.6,11.,5.4));
#23248=CARTESIAN_POINT('Origin',(1.,11.,4.5));
#23249=CARTESIAN_POINT('',(1.,11.,5.1));
#23250=CARTESIAN_POINT('',(1.,11.,5.1));
#23251=CARTESIAN_POINT('Origin',(1.,11.,4.5));
#23252=CARTESIAN_POINT('Origin',(21.5,11.,4.5));
#23253=CARTESIAN_POINT('',(21.5,11.,4.9));
#23254=CARTESIAN_POINT('Origin',(21.5,11.,4.5));
#23255=CARTESIAN_POINT('Origin',(21.5,11.,4.5));
#23256=CARTESIAN_POINT('',(23.5,11.,5.1));
#23257=CARTESIAN_POINT('Origin',(23.5,11.,4.5));
#23258=CARTESIAN_POINT('',(21.5,11.,5.1));
#23259=CARTESIAN_POINT('Origin',(3.5,11.,4.5));
#23260=CARTESIAN_POINT('',(3.5,11.,5.1));
#23261=CARTESIAN_POINT('Origin',(3.5,11.,4.5));
#23262=CARTESIAN_POINT('',(3.5,11.,4.9));
#23263=CARTESIAN_POINT('Origin',(3.5,11.,4.5));
#23264=CARTESIAN_POINT('Origin',(1.,11.,4.5));
#23265=CARTESIAN_POINT('',(1.,11.,5.1));
#23266=CARTESIAN_POINT('Origin',(1.,11.,4.5));
#23267=CARTESIAN_POINT('',(1.,11.,4.9));
#23268=CARTESIAN_POINT('Origin',(23.5,11.,4.5));
#23269=CARTESIAN_POINT('Origin',(1.,11.,4.5));
#23270=CARTESIAN_POINT('',(0.,0.,0.));
#23271=CARTESIAN_POINT('Origin',(0.4,11.,4.89));
#23272=CARTESIAN_POINT('',(0.260985612255421,10.9111180558268,4.89));
#23273=CARTESIAN_POINT('',(0.539014387744579,10.9111180558268,4.89));
#23274=CARTESIAN_POINT('',(-0.2,10.9111180558268,4.89));
#23275=CARTESIAN_POINT('Origin',(0.4,11.,4.89));
#23276=CARTESIAN_POINT('Origin',(0.4,11.,4.89));
#23277=CARTESIAN_POINT('',(0.260985612255421,11.0888819441732,4.89));
#23278=CARTESIAN_POINT('',(0.235,11.,4.9));
#23279=CARTESIAN_POINT('Ctrl Pts',(0.260985612255421,11.0888819441732,4.89));
#23280=CARTESIAN_POINT('Ctrl Pts',(0.255879904539473,11.08089644342,4.89181991495419));
#23281=CARTESIAN_POINT('Ctrl Pts',(0.251403608139787,11.0723643333024,4.89350251788328));
#23282=CARTESIAN_POINT('Ctrl Pts',(0.239243775830271,11.0431949313469,4.89819171553211));
#23283=CARTESIAN_POINT('Ctrl Pts',(0.235,11.0209808024963,4.9));
#23284=CARTESIAN_POINT('Ctrl Pts',(0.235,11.,4.9));
#23285=CARTESIAN_POINT('',(0.539014387744579,11.0888819441732,4.89));
#23286=CARTESIAN_POINT('Origin',(0.4,11.,4.89));
#23287=CARTESIAN_POINT('',(0.565,11.,4.9));
#23288=CARTESIAN_POINT('Ctrl Pts',(0.565,11.,4.9));
#23289=CARTESIAN_POINT('Ctrl Pts',(0.565,11.0209808024963,4.9));
#23290=CARTESIAN_POINT('Ctrl Pts',(0.560756224169729,11.0431949313469,4.89819171553211));
#23291=CARTESIAN_POINT('Ctrl Pts',(0.548596391860213,11.0723643333024,4.89350251788328));
#23292=CARTESIAN_POINT('Ctrl Pts',(0.544120095460527,11.08089644342,4.89181991495419));
#23293=CARTESIAN_POINT('Ctrl Pts',(0.539014387744579,11.0888819441732,4.89));
#23294=CARTESIAN_POINT('Ctrl Pts',(0.539014387744579,10.9111180558268,4.89));
#23295=CARTESIAN_POINT('Ctrl Pts',(0.544120095460527,10.91910355658,4.89181991495419));
#23296=CARTESIAN_POINT('Ctrl Pts',(0.548596391860213,10.9276356666976,4.89350251788328));
#23297=CARTESIAN_POINT('Ctrl Pts',(0.560756224169729,10.9568050686531,4.89819171553211));
#23298=CARTESIAN_POINT('Ctrl Pts',(0.565,10.9790191975037,4.9));
#23299=CARTESIAN_POINT('Ctrl Pts',(0.565,11.,4.9));
#23300=CARTESIAN_POINT('Ctrl Pts',(0.235,11.,4.9));
#23301=CARTESIAN_POINT('Ctrl Pts',(0.235,10.9790191975037,4.9));
#23302=CARTESIAN_POINT('Ctrl Pts',(0.239243775830271,10.9568050686531,4.89819171553211));
#23303=CARTESIAN_POINT('Ctrl Pts',(0.251403608139787,10.9276356666976,4.89350251788328));
#23304=CARTESIAN_POINT('Ctrl Pts',(0.255879904539473,10.91910355658,4.89181991495419));
#23305=CARTESIAN_POINT('Ctrl Pts',(0.260985612255421,10.9111180558268,4.89));
#23306=CARTESIAN_POINT('',(0.235,11.,6.));
#23307=CARTESIAN_POINT('',(0.235,11.,4.89));
#23308=CARTESIAN_POINT('',(0.4,10.835,5.99089738077441));
#23309=CARTESIAN_POINT('Ctrl Pts',(0.4,10.835,5.99089738077441));
#23310=CARTESIAN_POINT('Ctrl Pts',(0.379264160895016,10.835,5.99089738077441));
#23311=CARTESIAN_POINT('Ctrl Pts',(0.35715772909914,10.8391475009749,5.99137458218466));
#23312=CARTESIAN_POINT('Ctrl Pts',(0.316510155068951,10.8559915528391,5.99309518705251));
#23313=CARTESIAN_POINT('Ctrl Pts',(0.297967572401872,10.8686871898066,5.99431341615514));
#23314=CARTESIAN_POINT('Ctrl Pts',(0.268687262909328,10.8979674992991,5.99659781052538));
#23315=CARTESIAN_POINT('Ctrl Pts',(0.255991568780354,10.9165101139013,5.99781281581157));
#23316=CARTESIAN_POINT('Ctrl Pts',(0.239147474615801,10.9571577954068,5.99952603771524));
#23317=CARTESIAN_POINT('Ctrl Pts',(0.235,10.9792642644351,6.));
#23318=CARTESIAN_POINT('Ctrl Pts',(0.235,11.,6.));
#23319=CARTESIAN_POINT('',(0.565,11.,6.));
#23320=CARTESIAN_POINT('Ctrl Pts',(0.565,11.,6.));
#23321=CARTESIAN_POINT('Ctrl Pts',(0.565,10.9792642644351,6.));
#23322=CARTESIAN_POINT('Ctrl Pts',(0.5608525253842,10.9571577954068,5.99952603771524));
#23323=CARTESIAN_POINT('Ctrl Pts',(0.544008431219647,10.9165101139013,5.99781281581157));
#23324=CARTESIAN_POINT('Ctrl Pts',(0.531312737090672,10.8979674992991,5.99659781052538));
#23325=CARTESIAN_POINT('Ctrl Pts',(0.502032427598128,10.8686871898066,5.99431341615514));
#23326=CARTESIAN_POINT('Ctrl Pts',(0.483489844931049,10.8559915528391,5.99309518705251));
#23327=CARTESIAN_POINT('Ctrl Pts',(0.44284227090086,10.8391475009749,5.99137458218466));
#23328=CARTESIAN_POINT('Ctrl Pts',(0.420735839104984,10.835,5.99089738077441));
#23329=CARTESIAN_POINT('Ctrl Pts',(0.4,10.835,5.99089738077441));
#23330=CARTESIAN_POINT('Ctrl Pts',(0.235,11.,6.));
#23331=CARTESIAN_POINT('Ctrl Pts',(0.235,11.0207357355649,6.));
#23332=CARTESIAN_POINT('Ctrl Pts',(0.2391474746158,11.0428422045932,5.99952603771524));
#23333=CARTESIAN_POINT('Ctrl Pts',(0.255991568780353,11.0834898860987,5.99781281581157));
#23334=CARTESIAN_POINT('Ctrl Pts',(0.268687262909328,11.1020325007009,5.99659781052538));
#23335=CARTESIAN_POINT('Ctrl Pts',(0.297967572401872,11.1313128101934,5.99431341615514));
#23336=CARTESIAN_POINT('Ctrl Pts',(0.316510155068951,11.1440084471609,5.99309518705251));
#23337=CARTESIAN_POINT('Ctrl Pts',(0.35715772909914,11.1608524990251,5.99137458218466));
#23338=CARTESIAN_POINT('Ctrl Pts',(0.379264160895016,11.165,5.99089738077441));
#23339=CARTESIAN_POINT('Ctrl Pts',(0.420735839104984,11.165,5.99089738077441));
#23340=CARTESIAN_POINT('Ctrl Pts',(0.44284227090086,11.1608524990251,5.99137458218466));
#23341=CARTESIAN_POINT('Ctrl Pts',(0.483489844931049,11.1440084471609,5.99309518705251));
#23342=CARTESIAN_POINT('Ctrl Pts',(0.502032427598128,11.1313128101934,5.99431341615514));
#23343=CARTESIAN_POINT('Ctrl Pts',(0.531312737090672,11.1020325007009,5.99659781052538));
#23344=CARTESIAN_POINT('Ctrl Pts',(0.544008431219647,11.0834898860987,5.99781281581157));
#23345=CARTESIAN_POINT('Ctrl Pts',(0.5608525253842,11.0428422045932,5.99952603771524));
#23346=CARTESIAN_POINT('Ctrl Pts',(0.565,11.0207357355649,6.));
#23347=CARTESIAN_POINT('Ctrl Pts',(0.565,11.,6.));
#23348=CARTESIAN_POINT('Origin',(0.4,11.,4.89));
#23349=CARTESIAN_POINT('',(-0.2,11.0888819441732,4.89));
#23350=CARTESIAN_POINT('Origin',(-0.2,11.,4.5));
#23351=CARTESIAN_POINT('',(1.,11.,4.9));
#23352=CARTESIAN_POINT('Origin',(1.,11.,4.5));
#23353=CARTESIAN_POINT('',(-0.2,11.,4.9));
#23354=CARTESIAN_POINT('',(-0.2,11.,4.9));
#23355=CARTESIAN_POINT('',(-0.2,11.,4.9));
#23356=CARTESIAN_POINT('Origin',(-0.2,11.,4.5));
#23357=CARTESIAN_POINT('Origin',(-0.2,11.,4.5));
#23358=CARTESIAN_POINT('',(1.,11.,6.));
#23359=CARTESIAN_POINT('Origin',(1.,11.,4.5));
#23360=CARTESIAN_POINT('',(-0.2,11.,6.));
#23361=CARTESIAN_POINT('',(-0.2,11.,6.));
#23362=CARTESIAN_POINT('',(-0.2,11.,6.));
#23363=CARTESIAN_POINT('Origin',(-0.2,11.,4.5));
#23364=CARTESIAN_POINT('Origin',(1.,11.,4.5));
#23365=CARTESIAN_POINT('Origin',(-0.2,11.,4.5));
#23366=CARTESIAN_POINT('',(0.,0.,0.));
#23367=CARTESIAN_POINT('Origin',(0.0577350269189626,0.,-0.1));
#23368=CARTESIAN_POINT('',(0.0577350269189626,0.,-0.1));
#23369=CARTESIAN_POINT('',(0.115470053837925,0.,0.));
#23370=CARTESIAN_POINT('',(0.0934187836487032,0.,-0.0381939203391614));
#23371=CARTESIAN_POINT('',(0.0577350269189626,-0.2,-0.1));
#23372=CARTESIAN_POINT('',(0.0577350269189626,0.,-0.1));
#23373=CARTESIAN_POINT('',(0.115470053837925,-0.2,0.));
#23374=CARTESIAN_POINT('',(0.115470053837925,-0.2,0.));
#23375=CARTESIAN_POINT('',(0.115470053837925,0.,0.));
#23376=CARTESIAN_POINT('Origin',(-0.0577350269189626,0.,-0.1));
#23377=CARTESIAN_POINT('',(-0.0577350269189626,0.,-0.1));
#23378=CARTESIAN_POINT('',(0.0561324865405187,0.,-0.1));
#23379=CARTESIAN_POINT('',(-0.0577350269189626,-0.2,-0.1));
#23380=CARTESIAN_POINT('',(-0.0577350269189626,0.,-0.1));
#23381=CARTESIAN_POINT('',(0.0577350269189626,-0.2,-0.1));
#23382=CARTESIAN_POINT('Origin',(-0.115470053837925,0.,-1.38777878078145E-17));
#23383=CARTESIAN_POINT('',(-0.115470053837925,0.,-1.41410031829988E-17));
#23384=CARTESIAN_POINT('',(-0.0797862971081845,0.,-0.0618060796608387));
#23385=CARTESIAN_POINT('',(-0.115470053837925,-0.2,-1.38777878078145E-17));
#23386=CARTESIAN_POINT('',(-0.115470053837925,0.,-1.41410031829988E-17));
#23387=CARTESIAN_POINT('',(-0.0577350269189626,-0.2,-0.1));
#23388=CARTESIAN_POINT('Origin',(-0.0577350269189626,0.,0.1));
#23389=CARTESIAN_POINT('',(-0.0577350269189626,0.,0.1));
#23390=CARTESIAN_POINT('',(-0.0509187836487033,0.,0.111806079660839));
#23391=CARTESIAN_POINT('',(-0.0577350269189626,-0.2,0.1));
#23392=CARTESIAN_POINT('',(-0.0577350269189626,0.,0.1));
#23393=CARTESIAN_POINT('',(-0.115470053837925,-0.2,-1.41410031829988E-17));
#23394=CARTESIAN_POINT('Origin',(0.0577350269189626,0.,0.1));
#23395=CARTESIAN_POINT('',(0.0577350269189626,0.,0.1));
#23396=CARTESIAN_POINT('',(0.113867513459481,0.,0.1));
#23397=CARTESIAN_POINT('',(0.0577350269189626,-0.2,0.1));
#23398=CARTESIAN_POINT('',(0.0577350269189626,0.,0.1));
#23399=CARTESIAN_POINT('',(-0.0577350269189626,-0.2,0.1));
#23400=CARTESIAN_POINT('Origin',(0.115470053837925,0.,0.));
#23401=CARTESIAN_POINT('',(0.122286297108185,0.,-0.0118060796608386));
#23402=CARTESIAN_POINT('',(0.0577350269189626,-0.2,0.1));
#23403=CARTESIAN_POINT('Origin',(0.,-0.2,0.));
#23404=CARTESIAN_POINT('Origin',(0.17,0.,0.));
#23405=CARTESIAN_POINT('',(-0.17,-8.67361737988404E-18,-2.0818995585505E-17));
#23406=CARTESIAN_POINT('Origin',(0.,0.,0.));
#23407=CARTESIAN_POINT('Origin',(0.,-0.015,0.));
#23408=CARTESIAN_POINT('',(-0.1954,-0.0254,-2.39295984553393E-17));
#23409=CARTESIAN_POINT('Origin',(0.,-0.0254,0.));
#23410=CARTESIAN_POINT('',(-0.185,-0.015,-2.2655965784226E-17));
#23411=CARTESIAN_POINT('Origin',(0.,-0.2775,0.));
#23412=CARTESIAN_POINT('',(-0.1954,-0.5296,2.39295984553393E-17));
#23413=CARTESIAN_POINT('Origin',(0.,-0.5296,0.));
#23414=CARTESIAN_POINT('',(-0.1954,-0.2775,-2.39295984553393E-17));
#23415=CARTESIAN_POINT('Origin',(0.,-0.5625,0.));
#23416=CARTESIAN_POINT('',(-0.125,-0.6,-1.53080849893419E-17));
#23417=CARTESIAN_POINT('Origin',(0.,-0.6,0.));
#23418=CARTESIAN_POINT('',(-0.1625,-0.5625,-1.99005104861445E-17));
#23419=CARTESIAN_POINT('Origin',(0.,-0.6,0.));
#23420=CARTESIAN_POINT('',(0.,0.,0.));
#23421=CARTESIAN_POINT('',(0.,0.,0.));
#23422=CARTESIAN_POINT('',(0.,0.,0.));
#23423=CARTESIAN_POINT('',(0.,0.,0.));
#23424=CARTESIAN_POINT('',(0.,0.,0.));
#23425=CARTESIAN_POINT('',(0.,0.,0.));
#23426=CARTESIAN_POINT('',(0.,0.,0.));
#23427=CARTESIAN_POINT('',(0.,0.,0.));
#23428=CARTESIAN_POINT('',(10.,0.,0.));
#23429=CARTESIAN_POINT('',(8.5,-1.9,3.2));
#23430=CARTESIAN_POINT('',(8.5,1.9,3.2));
#23431=CARTESIAN_POINT('',(11.5,-1.9,3.2));
#23432=CARTESIAN_POINT('',(11.5,1.9,3.2));
#23433=CARTESIAN_POINT('',(7.2,-1.,4.));
#23434=CARTESIAN_POINT('',(7.2,1.,4.));
#23435=CARTESIAN_POINT('',(12.8,-1.,4.));
#23436=CARTESIAN_POINT('',(12.8,1.,4.));
#23437=CARTESIAN_POINT('',(10.,-0.9,7.));
#23438=CARTESIAN_POINT('',(10.,0.9,7.));
#23439=CARTESIAN_POINT('',(11.4142135623731,-2.1,8.4142135623731));
#23440=CARTESIAN_POINT('',(8.5857864376269,-2.1,8.4142135623731));
#23441=CARTESIAN_POINT('',(8.5857864376269,-2.1,5.58578643762691));
#23442=CARTESIAN_POINT('',(11.4142135623731,-2.1,5.58578643762691));
#23443=CARTESIAN_POINT('',(11.4142135623731,2.1,8.4142135623731));
#23444=CARTESIAN_POINT('',(8.5857864376269,2.1,8.4142135623731));
#23445=CARTESIAN_POINT('',(8.5857864376269,2.1,5.58578643762691));
#23446=CARTESIAN_POINT('',(11.4142135623731,2.1,5.58578643762691));
#23447=CARTESIAN_POINT('',(11.5,10.3,2.4));
#23448=CARTESIAN_POINT('',(12.5,11.7,2.4));
#23449=CARTESIAN_POINT('',(13.5,7.5,5.4));
#23450=CARTESIAN_POINT('',(0.,0.,0.));
#23451=CARTESIAN_POINT('',(0.,0.,0.));
#23452=CARTESIAN_POINT('',(0.4,11.,5.5));
#23453=CARTESIAN_POINT('',(0.,0.,0.));
#23454=CARTESIAN_POINT('',(0.,0.,0.));
#23455=CARTESIAN_POINT('',(0.,0.,0.));
#23456=CARTESIAN_POINT('',(0.,0.,0.));
#23457=CARTESIAN_POINT('',(0.,0.,0.));
#23458=UNCERTAINTY_MEASURE_WITH_UNIT(LENGTH_MEASURE(0.001),#23588,
'DISTANCE_ACCURACY_VALUE',
'Maximum model space distance between geometric entities at asserted c
onnectivities');
#23459=UNCERTAINTY_MEASURE_WITH_UNIT(LENGTH_MEASURE(0.001),#23588,
'DISTANCE_ACCURACY_VALUE',
'Maximum model space distance between geometric entities at asserted c
onnectivities');
#23460=UNCERTAINTY_MEASURE_WITH_UNIT(LENGTH_MEASURE(0.001),#23588,
'DISTANCE_ACCURACY_VALUE',
'Maximum model space distance between geometric entities at asserted c
onnectivities');
#23461=UNCERTAINTY_MEASURE_WITH_UNIT(LENGTH_MEASURE(0.001),#23588,
'DISTANCE_ACCURACY_VALUE',
'Maximum model space distance between geometric entities at asserted c
onnectivities');
#23462=UNCERTAINTY_MEASURE_WITH_UNIT(LENGTH_MEASURE(0.001),#23588,
'DISTANCE_ACCURACY_VALUE',
'Maximum model space distance between geometric entities at asserted c
onnectivities');
#23463=UNCERTAINTY_MEASURE_WITH_UNIT(LENGTH_MEASURE(0.001),#23588,
'DISTANCE_ACCURACY_VALUE',
'Maximum model space distance between geometric entities at asserted c
onnectivities');
#23464=UNCERTAINTY_MEASURE_WITH_UNIT(LENGTH_MEASURE(0.001),#23588,
'DISTANCE_ACCURACY_VALUE',
'Maximum model space distance between geometric entities at asserted c
onnectivities');
#23465=UNCERTAINTY_MEASURE_WITH_UNIT(LENGTH_MEASURE(0.001),#23588,
'DISTANCE_ACCURACY_VALUE',
'Maximum model space distance between geometric entities at asserted c
onnectivities');
#23466=UNCERTAINTY_MEASURE_WITH_UNIT(LENGTH_MEASURE(0.001),#23588,
'DISTANCE_ACCURACY_VALUE',
'Maximum model space distance between geometric entities at asserted c
onnectivities');
#23467=UNCERTAINTY_MEASURE_WITH_UNIT(LENGTH_MEASURE(0.001),#23588,
'DISTANCE_ACCURACY_VALUE',
'Maximum model space distance between geometric entities at asserted c
onnectivities');
#23468=UNCERTAINTY_MEASURE_WITH_UNIT(LENGTH_MEASURE(0.001),#23588,
'DISTANCE_ACCURACY_VALUE',
'Maximum model space distance between geometric entities at asserted c
onnectivities');
#23469=UNCERTAINTY_MEASURE_WITH_UNIT(LENGTH_MEASURE(0.001),#23588,
'DISTANCE_ACCURACY_VALUE',
'Maximum model space distance between geometric entities at asserted c
onnectivities');
#23470=UNCERTAINTY_MEASURE_WITH_UNIT(LENGTH_MEASURE(0.001),#23588,
'DISTANCE_ACCURACY_VALUE',
'Maximum model space distance between geometric entities at asserted c
onnectivities');
#23471=UNCERTAINTY_MEASURE_WITH_UNIT(LENGTH_MEASURE(0.001),#23588,
'DISTANCE_ACCURACY_VALUE',
'Maximum model space distance between geometric entities at asserted c
onnectivities');
#23472=UNCERTAINTY_MEASURE_WITH_UNIT(LENGTH_MEASURE(0.001),#23588,
'DISTANCE_ACCURACY_VALUE',
'Maximum model space distance between geometric entities at asserted c
onnectivities');
#23473=UNCERTAINTY_MEASURE_WITH_UNIT(LENGTH_MEASURE(0.001),#23588,
'DISTANCE_ACCURACY_VALUE',
'Maximum model space distance between geometric entities at asserted c
onnectivities');
#23474=UNCERTAINTY_MEASURE_WITH_UNIT(LENGTH_MEASURE(0.001),#23588,
'DISTANCE_ACCURACY_VALUE',
'Maximum model space distance between geometric entities at asserted c
onnectivities');
#23475=UNCERTAINTY_MEASURE_WITH_UNIT(LENGTH_MEASURE(0.001),#23588,
'DISTANCE_ACCURACY_VALUE',
'Maximum model space distance between geometric entities at asserted c
onnectivities');
#23476=UNCERTAINTY_MEASURE_WITH_UNIT(LENGTH_MEASURE(0.001),#23588,
'DISTANCE_ACCURACY_VALUE',
'Maximum model space distance between geometric entities at asserted c
onnectivities');
#23477=UNCERTAINTY_MEASURE_WITH_UNIT(LENGTH_MEASURE(0.001),#23588,
'DISTANCE_ACCURACY_VALUE',
'Maximum model space distance between geometric entities at asserted c
onnectivities');
#23478=UNCERTAINTY_MEASURE_WITH_UNIT(LENGTH_MEASURE(0.001),#23588,
'DISTANCE_ACCURACY_VALUE',
'Maximum model space distance between geometric entities at asserted c
onnectivities');
#23479=UNCERTAINTY_MEASURE_WITH_UNIT(LENGTH_MEASURE(0.001),#23588,
'DISTANCE_ACCURACY_VALUE',
'Maximum model space distance between geometric entities at asserted c
onnectivities');
#23480=UNCERTAINTY_MEASURE_WITH_UNIT(LENGTH_MEASURE(0.001),#23588,
'DISTANCE_ACCURACY_VALUE',
'Maximum model space distance between geometric entities at asserted c
onnectivities');
#23481=UNCERTAINTY_MEASURE_WITH_UNIT(LENGTH_MEASURE(0.001),#23588,
'DISTANCE_ACCURACY_VALUE',
'Maximum model space distance between geometric entities at asserted c
onnectivities');
#23482=UNCERTAINTY_MEASURE_WITH_UNIT(LENGTH_MEASURE(0.001),#23588,
'DISTANCE_ACCURACY_VALUE',
'Maximum model space distance between geometric entities at asserted c
onnectivities');
#23483=UNCERTAINTY_MEASURE_WITH_UNIT(LENGTH_MEASURE(0.001),#23588,
'DISTANCE_ACCURACY_VALUE',
'Maximum model space distance between geometric entities at asserted c
onnectivities');
#23484=UNCERTAINTY_MEASURE_WITH_UNIT(LENGTH_MEASURE(0.001),#23588,
'DISTANCE_ACCURACY_VALUE',
'Maximum model space distance between geometric entities at asserted c
onnectivities');
#23485=UNCERTAINTY_MEASURE_WITH_UNIT(LENGTH_MEASURE(0.001),#23588,
'DISTANCE_ACCURACY_VALUE',
'Maximum model space distance between geometric entities at asserted c
onnectivities');
#23486=UNCERTAINTY_MEASURE_WITH_UNIT(LENGTH_MEASURE(0.001),#23588,
'DISTANCE_ACCURACY_VALUE',
'Maximum model space distance between geometric entities at asserted c
onnectivities');
#23487=UNCERTAINTY_MEASURE_WITH_UNIT(LENGTH_MEASURE(0.001),#23588,
'DISTANCE_ACCURACY_VALUE',
'Maximum model space distance between geometric entities at asserted c
onnectivities');
#23488=UNCERTAINTY_MEASURE_WITH_UNIT(LENGTH_MEASURE(0.001),#23588,
'DISTANCE_ACCURACY_VALUE',
'Maximum model space distance between geometric entities at asserted c
onnectivities');
#23489=UNCERTAINTY_MEASURE_WITH_UNIT(LENGTH_MEASURE(0.001),#23588,
'DISTANCE_ACCURACY_VALUE',
'Maximum model space distance between geometric entities at asserted c
onnectivities');
#23490=UNCERTAINTY_MEASURE_WITH_UNIT(LENGTH_MEASURE(0.001),#23588,
'DISTANCE_ACCURACY_VALUE',
'Maximum model space distance between geometric entities at asserted c
onnectivities');
#23491=UNCERTAINTY_MEASURE_WITH_UNIT(LENGTH_MEASURE(0.001),#23588,
'DISTANCE_ACCURACY_VALUE',
'Maximum model space distance between geometric entities at asserted c
onnectivities');
#23492=UNCERTAINTY_MEASURE_WITH_UNIT(LENGTH_MEASURE(0.001),#23588,
'DISTANCE_ACCURACY_VALUE',
'Maximum model space distance between geometric entities at asserted c
onnectivities');
#23493=UNCERTAINTY_MEASURE_WITH_UNIT(LENGTH_MEASURE(0.001),#23588,
'DISTANCE_ACCURACY_VALUE',
'Maximum model space distance between geometric entities at asserted c
onnectivities');
#23494=UNCERTAINTY_MEASURE_WITH_UNIT(LENGTH_MEASURE(0.001),#23588,
'DISTANCE_ACCURACY_VALUE',
'Maximum model space distance between geometric entities at asserted c
onnectivities');
#23495=UNCERTAINTY_MEASURE_WITH_UNIT(LENGTH_MEASURE(0.001),#23588,
'DISTANCE_ACCURACY_VALUE',
'Maximum model space distance between geometric entities at asserted c
onnectivities');
#23496=UNCERTAINTY_MEASURE_WITH_UNIT(LENGTH_MEASURE(0.001),#23588,
'DISTANCE_ACCURACY_VALUE',
'Maximum model space distance between geometric entities at asserted c
onnectivities');
#23497=UNCERTAINTY_MEASURE_WITH_UNIT(LENGTH_MEASURE(0.001),#23588,
'DISTANCE_ACCURACY_VALUE',
'Maximum model space distance between geometric entities at asserted c
onnectivities');
#23498=UNCERTAINTY_MEASURE_WITH_UNIT(LENGTH_MEASURE(0.001),#23588,
'DISTANCE_ACCURACY_VALUE',
'Maximum model space distance between geometric entities at asserted c
onnectivities');
#23499=UNCERTAINTY_MEASURE_WITH_UNIT(LENGTH_MEASURE(0.001),#23588,
'DISTANCE_ACCURACY_VALUE',
'Maximum model space distance between geometric entities at asserted c
onnectivities');
#23500=UNCERTAINTY_MEASURE_WITH_UNIT(LENGTH_MEASURE(0.001),#23588,
'DISTANCE_ACCURACY_VALUE',
'Maximum model space distance between geometric entities at asserted c
onnectivities');
#23501=UNCERTAINTY_MEASURE_WITH_UNIT(LENGTH_MEASURE(0.001),#23588,
'DISTANCE_ACCURACY_VALUE',
'Maximum model space distance between geometric entities at asserted c
onnectivities');
#23502=UNCERTAINTY_MEASURE_WITH_UNIT(LENGTH_MEASURE(0.001),#23588,
'DISTANCE_ACCURACY_VALUE',
'Maximum model space distance between geometric entities at asserted c
onnectivities');
#23503=UNCERTAINTY_MEASURE_WITH_UNIT(LENGTH_MEASURE(0.001),#23588,
'DISTANCE_ACCURACY_VALUE',
'Maximum model space distance between geometric entities at asserted c
onnectivities');
#23504=UNCERTAINTY_MEASURE_WITH_UNIT(LENGTH_MEASURE(0.001),#23588,
'DISTANCE_ACCURACY_VALUE',
'Maximum model space distance between geometric entities at asserted c
onnectivities');
#23505=UNCERTAINTY_MEASURE_WITH_UNIT(LENGTH_MEASURE(0.001),#23588,
'DISTANCE_ACCURACY_VALUE',
'Maximum model space distance between geometric entities at asserted c
onnectivities');
#23506=UNCERTAINTY_MEASURE_WITH_UNIT(LENGTH_MEASURE(0.001),#23588,
'DISTANCE_ACCURACY_VALUE',
'Maximum model space distance between geometric entities at asserted c
onnectivities');
#23507=UNCERTAINTY_MEASURE_WITH_UNIT(LENGTH_MEASURE(0.001),#23588,
'DISTANCE_ACCURACY_VALUE',
'Maximum model space distance between geometric entities at asserted c
onnectivities');
#23508=UNCERTAINTY_MEASURE_WITH_UNIT(LENGTH_MEASURE(0.001),#23588,
'DISTANCE_ACCURACY_VALUE',
'Maximum model space distance between geometric entities at asserted c
onnectivities');
#23509=UNCERTAINTY_MEASURE_WITH_UNIT(LENGTH_MEASURE(0.001),#23588,
'DISTANCE_ACCURACY_VALUE',
'Maximum model space distance between geometric entities at asserted c
onnectivities');
#23510=UNCERTAINTY_MEASURE_WITH_UNIT(LENGTH_MEASURE(0.001),#23588,
'DISTANCE_ACCURACY_VALUE',
'Maximum model space distance between geometric entities at asserted c
onnectivities');
#23511=UNCERTAINTY_MEASURE_WITH_UNIT(LENGTH_MEASURE(0.001),#23588,
'DISTANCE_ACCURACY_VALUE',
'Maximum model space distance between geometric entities at asserted c
onnectivities');
#23512=UNCERTAINTY_MEASURE_WITH_UNIT(LENGTH_MEASURE(0.001),#23588,
'DISTANCE_ACCURACY_VALUE',
'Maximum model space distance between geometric entities at asserted c
onnectivities');
#23513=UNCERTAINTY_MEASURE_WITH_UNIT(LENGTH_MEASURE(0.001),#23588,
'DISTANCE_ACCURACY_VALUE',
'Maximum model space distance between geometric entities at asserted c
onnectivities');
#23514=UNCERTAINTY_MEASURE_WITH_UNIT(LENGTH_MEASURE(0.001),#23588,
'DISTANCE_ACCURACY_VALUE',
'Maximum model space distance between geometric entities at asserted c
onnectivities');
#23515=UNCERTAINTY_MEASURE_WITH_UNIT(LENGTH_MEASURE(0.001),#23588,
'DISTANCE_ACCURACY_VALUE',
'Maximum model space distance between geometric entities at asserted c
onnectivities');
#23516=UNCERTAINTY_MEASURE_WITH_UNIT(LENGTH_MEASURE(0.001),#23588,
'DISTANCE_ACCURACY_VALUE',
'Maximum model space distance between geometric entities at asserted c
onnectivities');
#23517=UNCERTAINTY_MEASURE_WITH_UNIT(LENGTH_MEASURE(0.001),#23588,
'DISTANCE_ACCURACY_VALUE',
'Maximum model space distance between geometric entities at asserted c
onnectivities');
#23518=UNCERTAINTY_MEASURE_WITH_UNIT(LENGTH_MEASURE(0.001),#23588,
'DISTANCE_ACCURACY_VALUE',
'Maximum model space distance between geometric entities at asserted c
onnectivities');
#23519=UNCERTAINTY_MEASURE_WITH_UNIT(LENGTH_MEASURE(0.001),#23588,
'DISTANCE_ACCURACY_VALUE',
'Maximum model space distance between geometric entities at asserted c
onnectivities');
#23520=UNCERTAINTY_MEASURE_WITH_UNIT(LENGTH_MEASURE(0.001),#23588,
'DISTANCE_ACCURACY_VALUE',
'Maximum model space distance between geometric entities at asserted c
onnectivities');
#23521=UNCERTAINTY_MEASURE_WITH_UNIT(LENGTH_MEASURE(0.001),#23588,
'DISTANCE_ACCURACY_VALUE',
'Maximum model space distance between geometric entities at asserted c
onnectivities');
#23522=UNCERTAINTY_MEASURE_WITH_UNIT(LENGTH_MEASURE(0.001),#23588,
'DISTANCE_ACCURACY_VALUE',
'Maximum model space distance between geometric entities at asserted c
onnectivities');
#23523=(
GEOMETRIC_REPRESENTATION_CONTEXT(3)
GLOBAL_UNCERTAINTY_ASSIGNED_CONTEXT((#23458))
GLOBAL_UNIT_ASSIGNED_CONTEXT((#23588,#23590,#23591))
REPRESENTATION_CONTEXT('','3D')
);
#23524=(
GEOMETRIC_REPRESENTATION_CONTEXT(3)
GLOBAL_UNCERTAINTY_ASSIGNED_CONTEXT((#23459))
GLOBAL_UNIT_ASSIGNED_CONTEXT((#23588,#23590,#23591))
REPRESENTATION_CONTEXT('','3D')
);
#23525=(
GEOMETRIC_REPRESENTATION_CONTEXT(3)
GLOBAL_UNCERTAINTY_ASSIGNED_CONTEXT((#23460))
GLOBAL_UNIT_ASSIGNED_CONTEXT((#23588,#23590,#23591))
REPRESENTATION_CONTEXT('','3D')
);
#23526=(
GEOMETRIC_REPRESENTATION_CONTEXT(3)
GLOBAL_UNCERTAINTY_ASSIGNED_CONTEXT((#23461))
GLOBAL_UNIT_ASSIGNED_CONTEXT((#23588,#23590,#23591))
REPRESENTATION_CONTEXT('','3D')
);
#23527=(
GEOMETRIC_REPRESENTATION_CONTEXT(3)
GLOBAL_UNCERTAINTY_ASSIGNED_CONTEXT((#23462))
GLOBAL_UNIT_ASSIGNED_CONTEXT((#23588,#23590,#23591))
REPRESENTATION_CONTEXT('','3D')
);
#23528=(
GEOMETRIC_REPRESENTATION_CONTEXT(3)
GLOBAL_UNCERTAINTY_ASSIGNED_CONTEXT((#23463))
GLOBAL_UNIT_ASSIGNED_CONTEXT((#23588,#23590,#23591))
REPRESENTATION_CONTEXT('','3D')
);
#23529=(
GEOMETRIC_REPRESENTATION_CONTEXT(3)
GLOBAL_UNCERTAINTY_ASSIGNED_CONTEXT((#23464))
GLOBAL_UNIT_ASSIGNED_CONTEXT((#23588,#23590,#23591))
REPRESENTATION_CONTEXT('','3D')
);
#23530=(
GEOMETRIC_REPRESENTATION_CONTEXT(3)
GLOBAL_UNCERTAINTY_ASSIGNED_CONTEXT((#23465))
GLOBAL_UNIT_ASSIGNED_CONTEXT((#23588,#23590,#23591))
REPRESENTATION_CONTEXT('','3D')
);
#23531=(
GEOMETRIC_REPRESENTATION_CONTEXT(3)
GLOBAL_UNCERTAINTY_ASSIGNED_CONTEXT((#23466))
GLOBAL_UNIT_ASSIGNED_CONTEXT((#23588,#23590,#23591))
REPRESENTATION_CONTEXT('','3D')
);
#23532=(
GEOMETRIC_REPRESENTATION_CONTEXT(3)
GLOBAL_UNCERTAINTY_ASSIGNED_CONTEXT((#23467))
GLOBAL_UNIT_ASSIGNED_CONTEXT((#23588,#23590,#23591))
REPRESENTATION_CONTEXT('','3D')
);
#23533=(
GEOMETRIC_REPRESENTATION_CONTEXT(3)
GLOBAL_UNCERTAINTY_ASSIGNED_CONTEXT((#23468))
GLOBAL_UNIT_ASSIGNED_CONTEXT((#23588,#23590,#23591))
REPRESENTATION_CONTEXT('','3D')
);
#23534=(
GEOMETRIC_REPRESENTATION_CONTEXT(3)
GLOBAL_UNCERTAINTY_ASSIGNED_CONTEXT((#23469))
GLOBAL_UNIT_ASSIGNED_CONTEXT((#23588,#23590,#23591))
REPRESENTATION_CONTEXT('','3D')
);
#23535=(
GEOMETRIC_REPRESENTATION_CONTEXT(3)
GLOBAL_UNCERTAINTY_ASSIGNED_CONTEXT((#23470))
GLOBAL_UNIT_ASSIGNED_CONTEXT((#23588,#23590,#23591))
REPRESENTATION_CONTEXT('','3D')
);
#23536=(
GEOMETRIC_REPRESENTATION_CONTEXT(3)
GLOBAL_UNCERTAINTY_ASSIGNED_CONTEXT((#23471))
GLOBAL_UNIT_ASSIGNED_CONTEXT((#23588,#23590,#23591))
REPRESENTATION_CONTEXT('','3D')
);
#23537=(
GEOMETRIC_REPRESENTATION_CONTEXT(3)
GLOBAL_UNCERTAINTY_ASSIGNED_CONTEXT((#23472))
GLOBAL_UNIT_ASSIGNED_CONTEXT((#23588,#23590,#23591))
REPRESENTATION_CONTEXT('','3D')
);
#23538=(
GEOMETRIC_REPRESENTATION_CONTEXT(3)
GLOBAL_UNCERTAINTY_ASSIGNED_CONTEXT((#23473))
GLOBAL_UNIT_ASSIGNED_CONTEXT((#23588,#23590,#23591))
REPRESENTATION_CONTEXT('','3D')
);
#23539=(
GEOMETRIC_REPRESENTATION_CONTEXT(3)
GLOBAL_UNCERTAINTY_ASSIGNED_CONTEXT((#23474))
GLOBAL_UNIT_ASSIGNED_CONTEXT((#23588,#23590,#23591))
REPRESENTATION_CONTEXT('','3D')
);
#23540=(
GEOMETRIC_REPRESENTATION_CONTEXT(3)
GLOBAL_UNCERTAINTY_ASSIGNED_CONTEXT((#23475))
GLOBAL_UNIT_ASSIGNED_CONTEXT((#23588,#23590,#23591))
REPRESENTATION_CONTEXT('','3D')
);
#23541=(
GEOMETRIC_REPRESENTATION_CONTEXT(3)
GLOBAL_UNCERTAINTY_ASSIGNED_CONTEXT((#23476))
GLOBAL_UNIT_ASSIGNED_CONTEXT((#23588,#23590,#23591))
REPRESENTATION_CONTEXT('','3D')
);
#23542=(
GEOMETRIC_REPRESENTATION_CONTEXT(3)
GLOBAL_UNCERTAINTY_ASSIGNED_CONTEXT((#23477))
GLOBAL_UNIT_ASSIGNED_CONTEXT((#23588,#23590,#23591))
REPRESENTATION_CONTEXT('','3D')
);
#23543=(
GEOMETRIC_REPRESENTATION_CONTEXT(3)
GLOBAL_UNCERTAINTY_ASSIGNED_CONTEXT((#23478))
GLOBAL_UNIT_ASSIGNED_CONTEXT((#23588,#23590,#23591))
REPRESENTATION_CONTEXT('','3D')
);
#23544=(
GEOMETRIC_REPRESENTATION_CONTEXT(3)
GLOBAL_UNCERTAINTY_ASSIGNED_CONTEXT((#23479))
GLOBAL_UNIT_ASSIGNED_CONTEXT((#23588,#23590,#23591))
REPRESENTATION_CONTEXT('','3D')
);
#23545=(
GEOMETRIC_REPRESENTATION_CONTEXT(3)
GLOBAL_UNCERTAINTY_ASSIGNED_CONTEXT((#23480))
GLOBAL_UNIT_ASSIGNED_CONTEXT((#23588,#23590,#23591))
REPRESENTATION_CONTEXT('','3D')
);
#23546=(
GEOMETRIC_REPRESENTATION_CONTEXT(3)
GLOBAL_UNCERTAINTY_ASSIGNED_CONTEXT((#23481))
GLOBAL_UNIT_ASSIGNED_CONTEXT((#23588,#23590,#23591))
REPRESENTATION_CONTEXT('','3D')
);
#23547=(
GEOMETRIC_REPRESENTATION_CONTEXT(3)
GLOBAL_UNCERTAINTY_ASSIGNED_CONTEXT((#23482))
GLOBAL_UNIT_ASSIGNED_CONTEXT((#23588,#23590,#23591))
REPRESENTATION_CONTEXT('','3D')
);
#23548=(
GEOMETRIC_REPRESENTATION_CONTEXT(3)
GLOBAL_UNCERTAINTY_ASSIGNED_CONTEXT((#23483))
GLOBAL_UNIT_ASSIGNED_CONTEXT((#23588,#23590,#23591))
REPRESENTATION_CONTEXT('','3D')
);
#23549=(
GEOMETRIC_REPRESENTATION_CONTEXT(3)
GLOBAL_UNCERTAINTY_ASSIGNED_CONTEXT((#23484))
GLOBAL_UNIT_ASSIGNED_CONTEXT((#23588,#23590,#23591))
REPRESENTATION_CONTEXT('','3D')
);
#23550=(
GEOMETRIC_REPRESENTATION_CONTEXT(3)
GLOBAL_UNCERTAINTY_ASSIGNED_CONTEXT((#23485))
GLOBAL_UNIT_ASSIGNED_CONTEXT((#23588,#23590,#23591))
REPRESENTATION_CONTEXT('','3D')
);
#23551=(
GEOMETRIC_REPRESENTATION_CONTEXT(3)
GLOBAL_UNCERTAINTY_ASSIGNED_CONTEXT((#23486))
GLOBAL_UNIT_ASSIGNED_CONTEXT((#23588,#23590,#23591))
REPRESENTATION_CONTEXT('','3D')
);
#23552=(
GEOMETRIC_REPRESENTATION_CONTEXT(3)
GLOBAL_UNCERTAINTY_ASSIGNED_CONTEXT((#23487))
GLOBAL_UNIT_ASSIGNED_CONTEXT((#23588,#23590,#23591))
REPRESENTATION_CONTEXT('','3D')
);
#23553=(
GEOMETRIC_REPRESENTATION_CONTEXT(3)
GLOBAL_UNCERTAINTY_ASSIGNED_CONTEXT((#23488))
GLOBAL_UNIT_ASSIGNED_CONTEXT((#23588,#23590,#23591))
REPRESENTATION_CONTEXT('','3D')
);
#23554=(
GEOMETRIC_REPRESENTATION_CONTEXT(3)
GLOBAL_UNCERTAINTY_ASSIGNED_CONTEXT((#23489))
GLOBAL_UNIT_ASSIGNED_CONTEXT((#23588,#23590,#23591))
REPRESENTATION_CONTEXT('','3D')
);
#23555=(
GEOMETRIC_REPRESENTATION_CONTEXT(3)
GLOBAL_UNCERTAINTY_ASSIGNED_CONTEXT((#23490))
GLOBAL_UNIT_ASSIGNED_CONTEXT((#23588,#23590,#23591))
REPRESENTATION_CONTEXT('','3D')
);
#23556=(
GEOMETRIC_REPRESENTATION_CONTEXT(3)
GLOBAL_UNCERTAINTY_ASSIGNED_CONTEXT((#23491))
GLOBAL_UNIT_ASSIGNED_CONTEXT((#23588,#23590,#23591))
REPRESENTATION_CONTEXT('','3D')
);
#23557=(
GEOMETRIC_REPRESENTATION_CONTEXT(3)
GLOBAL_UNCERTAINTY_ASSIGNED_CONTEXT((#23492))
GLOBAL_UNIT_ASSIGNED_CONTEXT((#23588,#23590,#23591))
REPRESENTATION_CONTEXT('','3D')
);
#23558=(
GEOMETRIC_REPRESENTATION_CONTEXT(3)
GLOBAL_UNCERTAINTY_ASSIGNED_CONTEXT((#23493))
GLOBAL_UNIT_ASSIGNED_CONTEXT((#23588,#23590,#23591))
REPRESENTATION_CONTEXT('','3D')
);
#23559=(
GEOMETRIC_REPRESENTATION_CONTEXT(3)
GLOBAL_UNCERTAINTY_ASSIGNED_CONTEXT((#23494))
GLOBAL_UNIT_ASSIGNED_CONTEXT((#23588,#23590,#23591))
REPRESENTATION_CONTEXT('','3D')
);
#23560=(
GEOMETRIC_REPRESENTATION_CONTEXT(3)
GLOBAL_UNCERTAINTY_ASSIGNED_CONTEXT((#23495))
GLOBAL_UNIT_ASSIGNED_CONTEXT((#23588,#23590,#23591))
REPRESENTATION_CONTEXT('','3D')
);
#23561=(
GEOMETRIC_REPRESENTATION_CONTEXT(3)
GLOBAL_UNCERTAINTY_ASSIGNED_CONTEXT((#23496))
GLOBAL_UNIT_ASSIGNED_CONTEXT((#23588,#23590,#23591))
REPRESENTATION_CONTEXT('','3D')
);
#23562=(
GEOMETRIC_REPRESENTATION_CONTEXT(3)
GLOBAL_UNCERTAINTY_ASSIGNED_CONTEXT((#23497))
GLOBAL_UNIT_ASSIGNED_CONTEXT((#23588,#23590,#23591))
REPRESENTATION_CONTEXT('','3D')
);
#23563=(
GEOMETRIC_REPRESENTATION_CONTEXT(3)
GLOBAL_UNCERTAINTY_ASSIGNED_CONTEXT((#23498))
GLOBAL_UNIT_ASSIGNED_CONTEXT((#23588,#23590,#23591))
REPRESENTATION_CONTEXT('','3D')
);
#23564=(
GEOMETRIC_REPRESENTATION_CONTEXT(3)
GLOBAL_UNCERTAINTY_ASSIGNED_CONTEXT((#23499))
GLOBAL_UNIT_ASSIGNED_CONTEXT((#23588,#23590,#23591))
REPRESENTATION_CONTEXT('','3D')
);
#23565=(
GEOMETRIC_REPRESENTATION_CONTEXT(3)
GLOBAL_UNCERTAINTY_ASSIGNED_CONTEXT((#23500))
GLOBAL_UNIT_ASSIGNED_CONTEXT((#23588,#23590,#23591))
REPRESENTATION_CONTEXT('','3D')
);
#23566=(
GEOMETRIC_REPRESENTATION_CONTEXT(3)
GLOBAL_UNCERTAINTY_ASSIGNED_CONTEXT((#23501))
GLOBAL_UNIT_ASSIGNED_CONTEXT((#23588,#23590,#23591))
REPRESENTATION_CONTEXT('','3D')
);
#23567=(
GEOMETRIC_REPRESENTATION_CONTEXT(3)
GLOBAL_UNCERTAINTY_ASSIGNED_CONTEXT((#23502))
GLOBAL_UNIT_ASSIGNED_CONTEXT((#23588,#23590,#23591))
REPRESENTATION_CONTEXT('','3D')
);
#23568=(
GEOMETRIC_REPRESENTATION_CONTEXT(3)
GLOBAL_UNCERTAINTY_ASSIGNED_CONTEXT((#23503))
GLOBAL_UNIT_ASSIGNED_CONTEXT((#23588,#23590,#23591))
REPRESENTATION_CONTEXT('','3D')
);
#23569=(
GEOMETRIC_REPRESENTATION_CONTEXT(3)
GLOBAL_UNCERTAINTY_ASSIGNED_CONTEXT((#23504))
GLOBAL_UNIT_ASSIGNED_CONTEXT((#23588,#23590,#23591))
REPRESENTATION_CONTEXT('','3D')
);
#23570=(
GEOMETRIC_REPRESENTATION_CONTEXT(3)
GLOBAL_UNCERTAINTY_ASSIGNED_CONTEXT((#23505))
GLOBAL_UNIT_ASSIGNED_CONTEXT((#23588,#23590,#23591))
REPRESENTATION_CONTEXT('','3D')
);
#23571=(
GEOMETRIC_REPRESENTATION_CONTEXT(3)
GLOBAL_UNCERTAINTY_ASSIGNED_CONTEXT((#23506))
GLOBAL_UNIT_ASSIGNED_CONTEXT((#23588,#23590,#23591))
REPRESENTATION_CONTEXT('','3D')
);
#23572=(
GEOMETRIC_REPRESENTATION_CONTEXT(3)
GLOBAL_UNCERTAINTY_ASSIGNED_CONTEXT((#23507))
GLOBAL_UNIT_ASSIGNED_CONTEXT((#23588,#23590,#23591))
REPRESENTATION_CONTEXT('','3D')
);
#23573=(
GEOMETRIC_REPRESENTATION_CONTEXT(3)
GLOBAL_UNCERTAINTY_ASSIGNED_CONTEXT((#23508))
GLOBAL_UNIT_ASSIGNED_CONTEXT((#23588,#23590,#23591))
REPRESENTATION_CONTEXT('','3D')
);
#23574=(
GEOMETRIC_REPRESENTATION_CONTEXT(3)
GLOBAL_UNCERTAINTY_ASSIGNED_CONTEXT((#23509))
GLOBAL_UNIT_ASSIGNED_CONTEXT((#23588,#23590,#23591))
REPRESENTATION_CONTEXT('','3D')
);
#23575=(
GEOMETRIC_REPRESENTATION_CONTEXT(3)
GLOBAL_UNCERTAINTY_ASSIGNED_CONTEXT((#23510))
GLOBAL_UNIT_ASSIGNED_CONTEXT((#23588,#23590,#23591))
REPRESENTATION_CONTEXT('','3D')
);
#23576=(
GEOMETRIC_REPRESENTATION_CONTEXT(3)
GLOBAL_UNCERTAINTY_ASSIGNED_CONTEXT((#23511))
GLOBAL_UNIT_ASSIGNED_CONTEXT((#23588,#23590,#23591))
REPRESENTATION_CONTEXT('','3D')
);
#23577=(
GEOMETRIC_REPRESENTATION_CONTEXT(3)
GLOBAL_UNCERTAINTY_ASSIGNED_CONTEXT((#23512))
GLOBAL_UNIT_ASSIGNED_CONTEXT((#23588,#23590,#23591))
REPRESENTATION_CONTEXT('','3D')
);
#23578=(
GEOMETRIC_REPRESENTATION_CONTEXT(3)
GLOBAL_UNCERTAINTY_ASSIGNED_CONTEXT((#23513))
GLOBAL_UNIT_ASSIGNED_CONTEXT((#23588,#23590,#23591))
REPRESENTATION_CONTEXT('','3D')
);
#23579=(
GEOMETRIC_REPRESENTATION_CONTEXT(3)
GLOBAL_UNCERTAINTY_ASSIGNED_CONTEXT((#23514))
GLOBAL_UNIT_ASSIGNED_CONTEXT((#23588,#23590,#23591))
REPRESENTATION_CONTEXT('','3D')
);
#23580=(
GEOMETRIC_REPRESENTATION_CONTEXT(3)
GLOBAL_UNCERTAINTY_ASSIGNED_CONTEXT((#23515))
GLOBAL_UNIT_ASSIGNED_CONTEXT((#23588,#23590,#23591))
REPRESENTATION_CONTEXT('','3D')
);
#23581=(
GEOMETRIC_REPRESENTATION_CONTEXT(3)
GLOBAL_UNCERTAINTY_ASSIGNED_CONTEXT((#23516))
GLOBAL_UNIT_ASSIGNED_CONTEXT((#23588,#23590,#23591))
REPRESENTATION_CONTEXT('','3D')
);
#23582=(
GEOMETRIC_REPRESENTATION_CONTEXT(3)
GLOBAL_UNCERTAINTY_ASSIGNED_CONTEXT((#23517))
GLOBAL_UNIT_ASSIGNED_CONTEXT((#23588,#23590,#23591))
REPRESENTATION_CONTEXT('','3D')
);
#23583=(
GEOMETRIC_REPRESENTATION_CONTEXT(3)
GLOBAL_UNCERTAINTY_ASSIGNED_CONTEXT((#23518))
GLOBAL_UNIT_ASSIGNED_CONTEXT((#23588,#23590,#23591))
REPRESENTATION_CONTEXT('','3D')
);
#23584=(
GEOMETRIC_REPRESENTATION_CONTEXT(3)
GLOBAL_UNCERTAINTY_ASSIGNED_CONTEXT((#23519))
GLOBAL_UNIT_ASSIGNED_CONTEXT((#23588,#23590,#23591))
REPRESENTATION_CONTEXT('','3D')
);
#23585=(
GEOMETRIC_REPRESENTATION_CONTEXT(3)
GLOBAL_UNCERTAINTY_ASSIGNED_CONTEXT((#23520))
GLOBAL_UNIT_ASSIGNED_CONTEXT((#23588,#23590,#23591))
REPRESENTATION_CONTEXT('','3D')
);
#23586=(
GEOMETRIC_REPRESENTATION_CONTEXT(3)
GLOBAL_UNCERTAINTY_ASSIGNED_CONTEXT((#23521))
GLOBAL_UNIT_ASSIGNED_CONTEXT((#23588,#23590,#23591))
REPRESENTATION_CONTEXT('','3D')
);
#23587=(
GEOMETRIC_REPRESENTATION_CONTEXT(3)
GLOBAL_UNCERTAINTY_ASSIGNED_CONTEXT((#23522))
GLOBAL_UNIT_ASSIGNED_CONTEXT((#23588,#23590,#23591))
REPRESENTATION_CONTEXT('','3D')
);
#23588=(
LENGTH_UNIT()
NAMED_UNIT(*)
SI_UNIT(.CENTI.,.METRE.)
);
#23589=(
LENGTH_UNIT()
NAMED_UNIT(*)
SI_UNIT($,.METRE.)
);
#23590=(
NAMED_UNIT(*)
PLANE_ANGLE_UNIT()
SI_UNIT($,.RADIAN.)
);
#23591=(
NAMED_UNIT(*)
SI_UNIT($,.STERADIAN.)
SOLID_ANGLE_UNIT()
);
#23592=SHAPE_DEFINITION_REPRESENTATION(#23656,#23825);
#23593=SHAPE_DEFINITION_REPRESENTATION(#23657,#23826);
#23594=SHAPE_DEFINITION_REPRESENTATION(#23658,#23827);
#23595=SHAPE_DEFINITION_REPRESENTATION(#23659,#23828);
#23596=SHAPE_DEFINITION_REPRESENTATION(#23660,#23829);
#23597=SHAPE_DEFINITION_REPRESENTATION(#23661,#23830);
#23598=SHAPE_DEFINITION_REPRESENTATION(#23662,#23831);
#23599=SHAPE_DEFINITION_REPRESENTATION(#23663,#23832);
#23600=SHAPE_DEFINITION_REPRESENTATION(#23664,#23833);
#23601=SHAPE_DEFINITION_REPRESENTATION(#23665,#23834);
#23602=SHAPE_DEFINITION_REPRESENTATION(#23666,#23835);
#23603=SHAPE_DEFINITION_REPRESENTATION(#23667,#23836);
#23604=SHAPE_DEFINITION_REPRESENTATION(#23668,#23837);
#23605=SHAPE_DEFINITION_REPRESENTATION(#23669,#23838);
#23606=SHAPE_DEFINITION_REPRESENTATION(#23670,#23839);
#23607=SHAPE_DEFINITION_REPRESENTATION(#23671,#23840);
#23608=SHAPE_DEFINITION_REPRESENTATION(#23672,#23841);
#23609=SHAPE_DEFINITION_REPRESENTATION(#23673,#23842);
#23610=SHAPE_DEFINITION_REPRESENTATION(#23674,#23843);
#23611=SHAPE_DEFINITION_REPRESENTATION(#23675,#23844);
#23612=SHAPE_DEFINITION_REPRESENTATION(#23676,#23845);
#23613=SHAPE_DEFINITION_REPRESENTATION(#23677,#23846);
#23614=SHAPE_DEFINITION_REPRESENTATION(#23683,#23847);
#23615=SHAPE_DEFINITION_REPRESENTATION(#23684,#23848);
#23616=SHAPE_DEFINITION_REPRESENTATION(#23685,#23849);
#23617=SHAPE_DEFINITION_REPRESENTATION(#23686,#23850);
#23618=SHAPE_DEFINITION_REPRESENTATION(#23687,#23851);
#23619=SHAPE_DEFINITION_REPRESENTATION(#23688,#23852);
#23620=SHAPE_DEFINITION_REPRESENTATION(#23689,#23853);
#23621=SHAPE_DEFINITION_REPRESENTATION(#23690,#23854);
#23622=SHAPE_DEFINITION_REPRESENTATION(#23691,#23855);
#23623=SHAPE_DEFINITION_REPRESENTATION(#23692,#23856);
#23624=SHAPE_DEFINITION_REPRESENTATION(#23693,#23857);
#23625=SHAPE_DEFINITION_REPRESENTATION(#23694,#23858);
#23626=SHAPE_DEFINITION_REPRESENTATION(#23695,#23859);
#23627=SHAPE_DEFINITION_REPRESENTATION(#23699,#23860);
#23628=SHAPE_DEFINITION_REPRESENTATION(#23700,#23861);
#23629=SHAPE_DEFINITION_REPRESENTATION(#23701,#23862);
#23630=SHAPE_DEFINITION_REPRESENTATION(#23702,#23863);
#23631=SHAPE_DEFINITION_REPRESENTATION(#23703,#23864);
#23632=SHAPE_DEFINITION_REPRESENTATION(#23704,#23865);
#23633=SHAPE_DEFINITION_REPRESENTATION(#23705,#23866);
#23634=SHAPE_DEFINITION_REPRESENTATION(#23711,#23867);
#23635=SHAPE_DEFINITION_REPRESENTATION(#23712,#23868);
#23636=SHAPE_DEFINITION_REPRESENTATION(#23713,#23869);
#23637=SHAPE_DEFINITION_REPRESENTATION(#23714,#23870);
#23638=SHAPE_DEFINITION_REPRESENTATION(#23715,#23871);
#23639=SHAPE_DEFINITION_REPRESENTATION(#23716,#23872);
#23640=SHAPE_DEFINITION_REPRESENTATION(#23717,#23873);
#23641=SHAPE_DEFINITION_REPRESENTATION(#23718,#23874);
#23642=SHAPE_DEFINITION_REPRESENTATION(#23719,#23875);
#23643=SHAPE_DEFINITION_REPRESENTATION(#23720,#23876);
#23644=SHAPE_DEFINITION_REPRESENTATION(#23721,#23877);
#23645=SHAPE_DEFINITION_REPRESENTATION(#23722,#23878);
#23646=SHAPE_DEFINITION_REPRESENTATION(#23723,#23879);
#23647=SHAPE_DEFINITION_REPRESENTATION(#23724,#23880);
#23648=SHAPE_DEFINITION_REPRESENTATION(#23725,#23881);
#23649=SHAPE_DEFINITION_REPRESENTATION(#23726,#23882);
#23650=SHAPE_DEFINITION_REPRESENTATION(#23727,#23883);
#23651=SHAPE_DEFINITION_REPRESENTATION(#23728,#23884);
#23652=SHAPE_DEFINITION_REPRESENTATION(#23783,#23885);
#23653=SHAPE_DEFINITION_REPRESENTATION(#23784,#23886);
#23654=SHAPE_DEFINITION_REPRESENTATION(#23785,#23887);
#23655=SHAPE_DEFINITION_REPRESENTATION(#23786,#23888);
#23656=PRODUCT_DEFINITION_SHAPE('',$,#23890);
#23657=PRODUCT_DEFINITION_SHAPE('',$,#23891);
#23658=PRODUCT_DEFINITION_SHAPE('',$,#23892);
#23659=PRODUCT_DEFINITION_SHAPE('',$,#23893);
#23660=PRODUCT_DEFINITION_SHAPE('',$,#23894);
#23661=PRODUCT_DEFINITION_SHAPE('',$,#23895);
#23662=PRODUCT_DEFINITION_SHAPE('',$,#23896);
#23663=PRODUCT_DEFINITION_SHAPE('',$,#23897);
#23664=PRODUCT_DEFINITION_SHAPE('',$,#23898);
#23665=PRODUCT_DEFINITION_SHAPE('',$,#23899);
#23666=PRODUCT_DEFINITION_SHAPE('',$,#23900);
#23667=PRODUCT_DEFINITION_SHAPE('',$,#23901);
#23668=PRODUCT_DEFINITION_SHAPE('',$,#23902);
#23669=PRODUCT_DEFINITION_SHAPE('',$,#23903);
#23670=PRODUCT_DEFINITION_SHAPE('',$,#23904);
#23671=PRODUCT_DEFINITION_SHAPE('',$,#23905);
#23672=PRODUCT_DEFINITION_SHAPE('',$,#23906);
#23673=PRODUCT_DEFINITION_SHAPE('',$,#23907);
#23674=PRODUCT_DEFINITION_SHAPE('',$,#23908);
#23675=PRODUCT_DEFINITION_SHAPE('',$,#23909);
#23676=PRODUCT_DEFINITION_SHAPE('',$,#23910);
#23677=PRODUCT_DEFINITION_SHAPE('',$,#23911);
#23678=PRODUCT_DEFINITION_SHAPE($,$,#332);
#23679=PRODUCT_DEFINITION_SHAPE($,$,#333);
#23680=PRODUCT_DEFINITION_SHAPE($,$,#334);
#23681=PRODUCT_DEFINITION_SHAPE($,$,#335);
#23682=PRODUCT_DEFINITION_SHAPE($,$,#336);
#23683=PRODUCT_DEFINITION_SHAPE('',$,#23912);
#23684=PRODUCT_DEFINITION_SHAPE('',$,#23913);
#23685=PRODUCT_DEFINITION_SHAPE('',$,#23914);
#23686=PRODUCT_DEFINITION_SHAPE('',$,#23915);
#23687=PRODUCT_DEFINITION_SHAPE('',$,#23916);
#23688=PRODUCT_DEFINITION_SHAPE('',$,#23917);
#23689=PRODUCT_DEFINITION_SHAPE('',$,#23918);
#23690=PRODUCT_DEFINITION_SHAPE('',$,#23919);
#23691=PRODUCT_DEFINITION_SHAPE('',$,#23920);
#23692=PRODUCT_DEFINITION_SHAPE('',$,#23921);
#23693=PRODUCT_DEFINITION_SHAPE('',$,#23922);
#23694=PRODUCT_DEFINITION_SHAPE('',$,#23923);
#23695=PRODUCT_DEFINITION_SHAPE('',$,#23924);
#23696=PRODUCT_DEFINITION_SHAPE($,$,#337);
#23697=PRODUCT_DEFINITION_SHAPE($,$,#338);
#23698=PRODUCT_DEFINITION_SHAPE($,$,#339);
#23699=PRODUCT_DEFINITION_SHAPE('',$,#23925);
#23700=PRODUCT_DEFINITION_SHAPE('',$,#23926);
#23701=PRODUCT_DEFINITION_SHAPE('',$,#23927);
#23702=PRODUCT_DEFINITION_SHAPE('',$,#23928);
#23703=PRODUCT_DEFINITION_SHAPE('',$,#23929);
#23704=PRODUCT_DEFINITION_SHAPE('',$,#23930);
#23705=PRODUCT_DEFINITION_SHAPE('',$,#23931);
#23706=PRODUCT_DEFINITION_SHAPE($,$,#340);
#23707=PRODUCT_DEFINITION_SHAPE($,$,#341);
#23708=PRODUCT_DEFINITION_SHAPE($,$,#342);
#23709=PRODUCT_DEFINITION_SHAPE($,$,#343);
#23710=PRODUCT_DEFINITION_SHAPE($,$,#344);
#23711=PRODUCT_DEFINITION_SHAPE('',$,#23932);
#23712=PRODUCT_DEFINITION_SHAPE('',$,#23933);
#23713=PRODUCT_DEFINITION_SHAPE('',$,#23934);
#23714=PRODUCT_DEFINITION_SHAPE('',$,#23935);
#23715=PRODUCT_DEFINITION_SHAPE('',$,#23936);
#23716=PRODUCT_DEFINITION_SHAPE('',$,#23937);
#23717=PRODUCT_DEFINITION_SHAPE('',$,#23938);
#23718=PRODUCT_DEFINITION_SHAPE('',$,#23939);
#23719=PRODUCT_DEFINITION_SHAPE('',$,#23940);
#23720=PRODUCT_DEFINITION_SHAPE('',$,#23941);
#23721=PRODUCT_DEFINITION_SHAPE('',$,#23942);
#23722=PRODUCT_DEFINITION_SHAPE('',$,#23943);
#23723=PRODUCT_DEFINITION_SHAPE('',$,#23944);
#23724=PRODUCT_DEFINITION_SHAPE('',$,#23945);
#23725=PRODUCT_DEFINITION_SHAPE('',$,#23946);
#23726=PRODUCT_DEFINITION_SHAPE('',$,#23947);
#23727=PRODUCT_DEFINITION_SHAPE('',$,#23948);
#23728=PRODUCT_DEFINITION_SHAPE('',$,#23949);
#23729=PRODUCT_DEFINITION_SHAPE($,$,#345);
#23730=PRODUCT_DEFINITION_SHAPE($,$,#346);
#23731=PRODUCT_DEFINITION_SHAPE($,$,#347);
#23732=PRODUCT_DEFINITION_SHAPE($,$,#348);
#23733=PRODUCT_DEFINITION_SHAPE($,$,#349);
#23734=PRODUCT_DEFINITION_SHAPE($,$,#350);
#23735=PRODUCT_DEFINITION_SHAPE($,$,#351);
#23736=PRODUCT_DEFINITION_SHAPE($,$,#352);
#23737=PRODUCT_DEFINITION_SHAPE($,$,#353);
#23738=PRODUCT_DEFINITION_SHAPE($,$,#354);
#23739=PRODUCT_DEFINITION_SHAPE($,$,#355);
#23740=PRODUCT_DEFINITION_SHAPE($,$,#356);
#23741=PRODUCT_DEFINITION_SHAPE($,$,#357);
#23742=PRODUCT_DEFINITION_SHAPE($,$,#358);
#23743=PRODUCT_DEFINITION_SHAPE($,$,#359);
#23744=PRODUCT_DEFINITION_SHAPE($,$,#360);
#23745=PRODUCT_DEFINITION_SHAPE($,$,#361);
#23746=PRODUCT_DEFINITION_SHAPE($,$,#362);
#23747=PRODUCT_DEFINITION_SHAPE($,$,#363);
#23748=PRODUCT_DEFINITION_SHAPE($,$,#364);
#23749=PRODUCT_DEFINITION_SHAPE($,$,#365);
#23750=PRODUCT_DEFINITION_SHAPE($,$,#366);
#23751=PRODUCT_DEFINITION_SHAPE($,$,#367);
#23752=PRODUCT_DEFINITION_SHAPE($,$,#368);
#23753=PRODUCT_DEFINITION_SHAPE($,$,#369);
#23754=PRODUCT_DEFINITION_SHAPE($,$,#370);
#23755=PRODUCT_DEFINITION_SHAPE($,$,#371);
#23756=PRODUCT_DEFINITION_SHAPE($,$,#372);
#23757=PRODUCT_DEFINITION_SHAPE($,$,#373);
#23758=PRODUCT_DEFINITION_SHAPE($,$,#374);
#23759=PRODUCT_DEFINITION_SHAPE($,$,#375);
#23760=PRODUCT_DEFINITION_SHAPE($,$,#376);
#23761=PRODUCT_DEFINITION_SHAPE($,$,#377);
#23762=PRODUCT_DEFINITION_SHAPE($,$,#378);
#23763=PRODUCT_DEFINITION_SHAPE($,$,#379);
#23764=PRODUCT_DEFINITION_SHAPE($,$,#380);
#23765=PRODUCT_DEFINITION_SHAPE($,$,#381);
#23766=PRODUCT_DEFINITION_SHAPE($,$,#382);
#23767=PRODUCT_DEFINITION_SHAPE($,$,#383);
#23768=PRODUCT_DEFINITION_SHAPE($,$,#384);
#23769=PRODUCT_DEFINITION_SHAPE($,$,#385);
#23770=PRODUCT_DEFINITION_SHAPE($,$,#386);
#23771=PRODUCT_DEFINITION_SHAPE($,$,#387);
#23772=PRODUCT_DEFINITION_SHAPE($,$,#388);
#23773=PRODUCT_DEFINITION_SHAPE($,$,#389);
#23774=PRODUCT_DEFINITION_SHAPE($,$,#390);
#23775=PRODUCT_DEFINITION_SHAPE($,$,#391);
#23776=PRODUCT_DEFINITION_SHAPE($,$,#392);
#23777=PRODUCT_DEFINITION_SHAPE($,$,#393);
#23778=PRODUCT_DEFINITION_SHAPE($,$,#394);
#23779=PRODUCT_DEFINITION_SHAPE($,$,#395);
#23780=PRODUCT_DEFINITION_SHAPE($,$,#396);
#23781=PRODUCT_DEFINITION_SHAPE($,$,#397);
#23782=PRODUCT_DEFINITION_SHAPE($,$,#398);
#23783=PRODUCT_DEFINITION_SHAPE('',$,#23950);
#23784=PRODUCT_DEFINITION_SHAPE('',$,#23951);
#23785=PRODUCT_DEFINITION_SHAPE('',$,#23952);
#23786=PRODUCT_DEFINITION_SHAPE('',$,#23953);
#23787=PRODUCT_DEFINITION_SHAPE($,$,#399);
#23788=PRODUCT_DEFINITION_SHAPE($,$,#400);
#23789=PRODUCT_DEFINITION_SHAPE($,$,#401);
#23790=PRODUCT_DEFINITION_SHAPE($,$,#402);
#23791=PRODUCT_DEFINITION_SHAPE($,$,#403);
#23792=PRODUCT_DEFINITION_SHAPE($,$,#404);
#23793=PRODUCT_DEFINITION_SHAPE($,$,#405);
#23794=PRODUCT_DEFINITION_SHAPE($,$,#406);
#23795=PRODUCT_DEFINITION_SHAPE($,$,#407);
#23796=PRODUCT_DEFINITION_SHAPE($,$,#408);
#23797=PRODUCT_DEFINITION_SHAPE($,$,#409);
#23798=PRODUCT_DEFINITION_SHAPE($,$,#410);
#23799=PRODUCT_DEFINITION_SHAPE($,$,#411);
#23800=PRODUCT_DEFINITION_SHAPE($,$,#412);
#23801=PRODUCT_DEFINITION_SHAPE($,$,#413);
#23802=PRODUCT_DEFINITION_SHAPE($,$,#414);
#23803=PRODUCT_DEFINITION_SHAPE($,$,#415);
#23804=PRODUCT_DEFINITION_SHAPE($,$,#416);
#23805=PRODUCT_DEFINITION_SHAPE($,$,#417);
#23806=PRODUCT_DEFINITION_SHAPE($,$,#418);
#23807=PRODUCT_DEFINITION_SHAPE($,$,#419);
#23808=PRODUCT_DEFINITION_SHAPE($,$,#420);
#23809=PRODUCT_DEFINITION_SHAPE($,$,#421);
#23810=PRODUCT_DEFINITION_SHAPE($,$,#422);
#23811=PRODUCT_DEFINITION_SHAPE($,$,#423);
#23812=PRODUCT_DEFINITION_SHAPE($,$,#424);
#23813=PRODUCT_DEFINITION_SHAPE($,$,#425);
#23814=PRODUCT_DEFINITION_SHAPE($,$,#426);
#23815=PRODUCT_DEFINITION_SHAPE($,$,#427);
#23816=PRODUCT_DEFINITION_SHAPE($,$,#428);
#23817=PRODUCT_DEFINITION_SHAPE($,$,#429);
#23818=PRODUCT_DEFINITION_SHAPE($,$,#430);
#23819=PRODUCT_DEFINITION_SHAPE($,$,#431);
#23820=PRODUCT_DEFINITION_SHAPE($,$,#432);
#23821=PRODUCT_DEFINITION_SHAPE($,$,#433);
#23822=PRODUCT_DEFINITION_SHAPE($,$,#434);
#23823=PRODUCT_DEFINITION_SHAPE($,$,#435);
#23824=PRODUCT_DEFINITION_SHAPE($,$,#436);
#23825=SHAPE_REPRESENTATION('',(#12876,#14512,#14513,#14514,#14515,#14516),
#23523);
#23826=SHAPE_REPRESENTATION('',(#12877,#14359,#14360,#14361,#14362,#14363,
#14364,#14365,#14366,#14367,#14368,#14369,#14370,#14371,#14372,#14373,#14374,
#14375,#14376,#14377,#14378,#14379,#14380,#14381,#14382,#14383,#14384,#14385,
#14386,#14387,#14388,#14389,#14390,#14391,#14392,#14393,#14394,#14395,#14396),
#23524);
#23827=SHAPE_REPRESENTATION('',(#12878),#23525);
#23828=SHAPE_REPRESENTATION('',(#12941),#23526);
#23829=SHAPE_REPRESENTATION('',(#12948),#23527);
#23830=SHAPE_REPRESENTATION('',(#12955),#23528);
#23831=SHAPE_REPRESENTATION('',(#12993),#23529);
#23832=SHAPE_REPRESENTATION('',(#13002),#23530);
#23833=SHAPE_REPRESENTATION('',(#13036),#23531);
#23834=SHAPE_REPRESENTATION('',(#13070),#23532);
#23835=SHAPE_REPRESENTATION('',(#13094),#23533);
#23836=SHAPE_REPRESENTATION('',(#13103),#23534);
#23837=SHAPE_REPRESENTATION('',(#13127),#23535);
#23838=SHAPE_REPRESENTATION('',(#13136),#23536);
#23839=SHAPE_REPRESENTATION('',(#13145),#23537);
#23840=SHAPE_REPRESENTATION('',(#13178),#23538);
#23841=SHAPE_REPRESENTATION('',(#13221,#13350,#13351,#13352,#13353,#13354),
#23539);
#23842=SHAPE_REPRESENTATION('',(#13222),#23540);
#23843=SHAPE_REPRESENTATION('',(#13242),#23541);
#23844=SHAPE_REPRESENTATION('',(#13262),#23542);
#23845=SHAPE_REPRESENTATION('',(#13279),#23543);
#23846=SHAPE_REPRESENTATION('',(#13333),#23544);
#23847=SHAPE_REPRESENTATION('',(#13355,#14479,#14480,#14481,#14482,#14483,
#14484,#14485,#14486,#14487,#14488,#14489,#14490,#14491,#14492,#14493,#14494,
#14495,#14496,#14497,#14498,#14499,#14500,#14501,#14502,#14503,#14504,#14505,
#14506,#14507,#14508),#23545);
#23848=SHAPE_REPRESENTATION('',(#13356),#23546);
#23849=SHAPE_REPRESENTATION('',(#13393),#23547);
#23850=SHAPE_REPRESENTATION('',(#13447),#23548);
#23851=SHAPE_REPRESENTATION('',(#13456),#23549);
#23852=SHAPE_REPRESENTATION('',(#13490),#23550);
#23853=SHAPE_REPRESENTATION('',(#13524),#23551);
#23854=SHAPE_REPRESENTATION('',(#13542),#23552);
#23855=SHAPE_REPRESENTATION('',(#13548),#23553);
#23856=SHAPE_REPRESENTATION('',(#13564,#13626,#13627,#13628),#23554);
#23857=SHAPE_REPRESENTATION('',(#13565),#23555);
#23858=SHAPE_REPRESENTATION('',(#13604),#23556);
#23859=SHAPE_REPRESENTATION('',(#13615),#23557);
#23860=SHAPE_REPRESENTATION('',(#13629),#23558);
#23861=SHAPE_REPRESENTATION('',(#13653,#13776,#13777,#13778,#13779,#13780),
#23559);
#23862=SHAPE_REPRESENTATION('',(#13654),#23560);
#23863=SHAPE_REPRESENTATION('',(#13674),#23561);
#23864=SHAPE_REPRESENTATION('',(#13694),#23562);
#23865=SHAPE_REPRESENTATION('',(#13709),#23563);
#23866=SHAPE_REPRESENTATION('',(#13759),#23564);
#23867=SHAPE_REPRESENTATION('',(#13781),#23565);
#23868=SHAPE_REPRESENTATION('',(#13805,#14397,#14398,#14399,#14400,#14401,
#14402,#14403,#14404),#23566);
#23869=SHAPE_REPRESENTATION('',(#13806),#23567);
#23870=SHAPE_REPRESENTATION('',(#13828),#23568);
#23871=SHAPE_REPRESENTATION('',(#13841),#23569);
#23872=SHAPE_REPRESENTATION('',(#13850),#23570);
#23873=SHAPE_REPRESENTATION('',(#13856),#23571);
#23874=SHAPE_REPRESENTATION('',(#13862),#23572);
#23875=SHAPE_REPRESENTATION('',(#13871),#23573);
#23876=SHAPE_REPRESENTATION('',(#14013,#14405,#14406,#14407,#14408,#14409,
#14410,#14411,#14412),#23574);
#23877=SHAPE_REPRESENTATION('',(#14014),#23575);
#23878=SHAPE_REPRESENTATION('',(#14032),#23576);
#23879=SHAPE_REPRESENTATION('',(#14041),#23577);
#23880=SHAPE_REPRESENTATION('',(#14050),#23578);
#23881=SHAPE_REPRESENTATION('',(#14056),#23579);
#23882=SHAPE_REPRESENTATION('',(#14062),#23580);
#23883=SHAPE_REPRESENTATION('',(#14071),#23581);
#23884=SHAPE_REPRESENTATION('',(#14333),#23582);
#23885=SHAPE_REPRESENTATION('',(#14413,#14509,#14510,#14511),#23583);
#23886=SHAPE_REPRESENTATION('',(#14414),#23584);
#23887=SHAPE_REPRESENTATION('',(#14448),#23585);
#23888=SHAPE_REPRESENTATION('',(#14462),#23586);
#23889=PRODUCT_DEFINITION_CONTEXT('part definition',#24083,'design');
#23890=PRODUCT_DEFINITION('PAT-011','PAT-011',#23954,
#23889);
#23891=PRODUCT_DEFINITION('Base and guide','Base and guide',#23955,#23889);
#23892=PRODUCT_DEFINITION('Base','Base',#23956,#23889);
#23893=PRODUCT_DEFINITION('Foot','Foot',#23957,#23889);
#23894=PRODUCT_DEFINITION('Foot (1)','Foot (1)',#23958,#23889);
#23895=PRODUCT_DEFINITION('Fixed bearing block','Fixed bearing block',#23959,
#23889);
#23896=PRODUCT_DEFINITION('Input outer spacer','Input outer spacer',#23960,
#23889);
#23897=PRODUCT_DEFINITION('Input bearing cap','Input bearing cap',#23961,
#23889);
#23898=PRODUCT_DEFINITION('Input bearing cap (1)','Input bearing cap (1)',
#23962,#23889);
#23899=PRODUCT_DEFINITION('Screw support','Screw support',#23963,#23889);
#23900=PRODUCT_DEFINITION('Screw bushing','Screw bushing',#23964,#23889);
#23901=PRODUCT_DEFINITION('Screw support (1)','Screw support (1)',#23965,
#23889);
#23902=PRODUCT_DEFINITION('Screw bushing (1)','Screw bushing (1)',#23966,
#23889);
#23903=PRODUCT_DEFINITION('Force gauge envelope','Force gauge envelope',
#23967,#23889);
#23904=PRODUCT_DEFINITION('Gauge mounting saddle',
'Gauge mounting saddle',#23968,#23889);
#23905=PRODUCT_DEFINITION('Linear Guide Rail - 15 mm, 220 mm Long',
'Linear Guide Rail - 15 mm, 220 mm Long',#23969,#23889);
#23906=PRODUCT_DEFINITION('Sealed Ball Bearing - 10 x 30 x 9 mm',
'Sealed Ball Bearing - 10 x 30 x 9 mm',#23970,#23889);
#23907=PRODUCT_DEFINITION('Inner ring','Inner ring',#23971,#23889);
#23908=PRODUCT_DEFINITION('Outer ring','Outer ring',#23972,#23889);
#23909=PRODUCT_DEFINITION('Balls','Balls',#23973,#23889);
#23910=PRODUCT_DEFINITION('Cage','Cage',#23974,#23889);
#23911=PRODUCT_DEFINITION('Seals 2RS','Seals 2RS',#23975,#23889);
#23912=PRODUCT_DEFINITION('Sliding bearing and gauge rod',
'Sliding bearing and gauge rod',#23976,#23889);
#23913=PRODUCT_DEFINITION('Sliding plate','Sliding plate',#23977,#23889);
#23914=PRODUCT_DEFINITION('Sliding bearing block',
'Sliding bearing block',#23978,#23889);
#23915=PRODUCT_DEFINITION('Output outer spacer','Output outer spacer',#23979,
#23889);
#23916=PRODUCT_DEFINITION('Output bearing cap','Output bearing cap',#23980,
#23889);
#23917=PRODUCT_DEFINITION('Output bearing cap (1)',
'Output bearing cap (1)',#23981,#23889);
#23918=PRODUCT_DEFINITION('Adjusting nut pedestal',
'Adjusting nut pedestal',#23982,#23889);
#23919=PRODUCT_DEFINITION('Gauge extension rod','Gauge extension rod',#23983,
#23889);
#23920=PRODUCT_DEFINITION('Gauge rod bracket','Gauge rod bracket',#23984,
#23889);
#23921=PRODUCT_DEFINITION('Flanged Linear Guide Carriage - 15 mm',
'Flanged Linear Guide Carriage - 15 mm',#23985,#23889);
#23922=PRODUCT_DEFINITION('Block','Block',#23986,#23889);
#23923=PRODUCT_DEFINITION('End cap +','End cap +',#23987,#23889);
#23924=PRODUCT_DEFINITION('End cap','End cap',#23988,#23889);
#23925=PRODUCT_DEFINITION('M5x14 Cap Screw','M5x14 Cap Screw',#23989,#23889);
#23926=PRODUCT_DEFINITION('Sealed Ball Bearing - 12 x 32 x 10 mm',
'Sealed Ball Bearing - 12 x 32 x 10 mm',#23990,#23889);
#23927=PRODUCT_DEFINITION('Inner ring (1)','Inner ring (1)',#23991,#23889);
#23928=PRODUCT_DEFINITION('Outer ring (1)','Outer ring (1)',#23992,#23889);
#23929=PRODUCT_DEFINITION('Balls (1)','Balls (1)',#23993,#23889);
#23930=PRODUCT_DEFINITION('Cage (1)','Cage (1)',#23994,#23889);
#23931=PRODUCT_DEFINITION('Seals 2RS (1)','Seals 2RS (1)',#23995,#23889);
#23932=PRODUCT_DEFINITION('M4x10 Cap Screw','M4x10 Cap Screw',#23996,#23889);
#23933=PRODUCT_DEFINITION('Input pulley','Input pulley',#23997,#23889);
#23934=PRODUCT_DEFINITION('Input shaft','Input shaft',#23998,#23889);
#23935=PRODUCT_DEFINITION('Input inner spacer','Input inner spacer',#23999,
#23889);
#23936=PRODUCT_DEFINITION('Input inner sleeve','Input inner sleeve',#24000,
#23889);
#23937=PRODUCT_DEFINITION('Input M3 set screw','Input M3 set screw',#24001,
#23889);
#23938=PRODUCT_DEFINITION('Input M3 set screw (1)',
'Input M3 set screw (1)',#24002,#23889);
#23939=PRODUCT_DEFINITION('Input end keeper','Input end keeper',#24003,
#23889);
#23940=PRODUCT_DEFINITION(
'Timing Pulley - 2 mm Pitch, 20 Teeth, 8 mm Bore',
'Timing Pulley - 2 mm Pitch, 20 Teeth, 8 mm Bore',#24004,#23889);
#23941=PRODUCT_DEFINITION('Sliding pulley','Sliding pulley',#24005,#23889);
#23942=PRODUCT_DEFINITION('Output shaft','Output shaft',#24006,#23889);
#23943=PRODUCT_DEFINITION('Output inner spacer','Output inner spacer',#24007,
#23889);
#23944=PRODUCT_DEFINITION('Output inner sleeve','Output inner sleeve',#24008,
#23889);
#23945=PRODUCT_DEFINITION('Output M3 set screw','Output M3 set screw',#24009,
#23889);
#23946=PRODUCT_DEFINITION('Output M3 set screw (1)',
'Output M3 set screw (1)',#24010,#23889);
#23947=PRODUCT_DEFINITION('Output end keeper','Output end keeper',#24011,
#23889);
#23948=PRODUCT_DEFINITION(
'Timing Pulley - 2 mm Pitch, 40 Teeth, 12 mm Bore',
'Timing Pulley - 2 mm Pitch, 40 Teeth, 12 mm Bore',#24012,#23889);
#23949=PRODUCT_DEFINITION('Cap Screw - M4x16','Cap Screw - M4x16',#24013,
#23889);
#23950=PRODUCT_DEFINITION('Adjusting screw','Adjusting screw',#24014,#23889);
#23951=PRODUCT_DEFINITION('M8x1.25 adjusting spindle',
'M8x1.25 adjusting spindle',#24015,#23889);
#23952=PRODUCT_DEFINITION('Adjusting knob','Adjusting knob',#24016,#23889);
#23953=PRODUCT_DEFINITION('Socket Set Screw - M4x6',
'Socket Set Screw - M4x6',#24017,#23889);
#23954=PRODUCT_DEFINITION_FORMATION('',$,#24085);
#23955=PRODUCT_DEFINITION_FORMATION('',$,#24086);
#23956=PRODUCT_DEFINITION_FORMATION('',$,#24087);
#23957=PRODUCT_DEFINITION_FORMATION('',$,#24088);
#23958=PRODUCT_DEFINITION_FORMATION('',$,#24089);
#23959=PRODUCT_DEFINITION_FORMATION('',$,#24090);
#23960=PRODUCT_DEFINITION_FORMATION('',$,#24091);
#23961=PRODUCT_DEFINITION_FORMATION('',$,#24092);
#23962=PRODUCT_DEFINITION_FORMATION('',$,#24093);
#23963=PRODUCT_DEFINITION_FORMATION('',$,#24094);
#23964=PRODUCT_DEFINITION_FORMATION('',$,#24095);
#23965=PRODUCT_DEFINITION_FORMATION('',$,#24096);
#23966=PRODUCT_DEFINITION_FORMATION('',$,#24097);
#23967=PRODUCT_DEFINITION_FORMATION('',$,#24098);
#23968=PRODUCT_DEFINITION_FORMATION('',$,#24099);
#23969=PRODUCT_DEFINITION_FORMATION('',$,#24100);
#23970=PRODUCT_DEFINITION_FORMATION('',$,#24101);
#23971=PRODUCT_DEFINITION_FORMATION('',$,#24102);
#23972=PRODUCT_DEFINITION_FORMATION('',$,#24103);
#23973=PRODUCT_DEFINITION_FORMATION('',$,#24104);
#23974=PRODUCT_DEFINITION_FORMATION('',$,#24105);
#23975=PRODUCT_DEFINITION_FORMATION('',$,#24106);
#23976=PRODUCT_DEFINITION_FORMATION('',$,#24107);
#23977=PRODUCT_DEFINITION_FORMATION('',$,#24108);
#23978=PRODUCT_DEFINITION_FORMATION('',$,#24109);
#23979=PRODUCT_DEFINITION_FORMATION('',$,#24110);
#23980=PRODUCT_DEFINITION_FORMATION('',$,#24111);
#23981=PRODUCT_DEFINITION_FORMATION('',$,#24112);
#23982=PRODUCT_DEFINITION_FORMATION('',$,#24113);
#23983=PRODUCT_DEFINITION_FORMATION('',$,#24114);
#23984=PRODUCT_DEFINITION_FORMATION('',$,#24115);
#23985=PRODUCT_DEFINITION_FORMATION('',$,#24116);
#23986=PRODUCT_DEFINITION_FORMATION('',$,#24117);
#23987=PRODUCT_DEFINITION_FORMATION('',$,#24118);
#23988=PRODUCT_DEFINITION_FORMATION('',$,#24119);
#23989=PRODUCT_DEFINITION_FORMATION('',$,#24120);
#23990=PRODUCT_DEFINITION_FORMATION('',$,#24121);
#23991=PRODUCT_DEFINITION_FORMATION('',$,#24122);
#23992=PRODUCT_DEFINITION_FORMATION('',$,#24123);
#23993=PRODUCT_DEFINITION_FORMATION('',$,#24124);
#23994=PRODUCT_DEFINITION_FORMATION('',$,#24125);
#23995=PRODUCT_DEFINITION_FORMATION('',$,#24126);
#23996=PRODUCT_DEFINITION_FORMATION('',$,#24127);
#23997=PRODUCT_DEFINITION_FORMATION('',$,#24128);
#23998=PRODUCT_DEFINITION_FORMATION('',$,#24129);
#23999=PRODUCT_DEFINITION_FORMATION('',$,#24130);
#24000=PRODUCT_DEFINITION_FORMATION('',$,#24131);
#24001=PRODUCT_DEFINITION_FORMATION('',$,#24132);
#24002=PRODUCT_DEFINITION_FORMATION('',$,#24133);
#24003=PRODUCT_DEFINITION_FORMATION('',$,#24134);
#24004=PRODUCT_DEFINITION_FORMATION('',$,#24135);
#24005=PRODUCT_DEFINITION_FORMATION('',$,#24136);
#24006=PRODUCT_DEFINITION_FORMATION('',$,#24137);
#24007=PRODUCT_DEFINITION_FORMATION('',$,#24138);
#24008=PRODUCT_DEFINITION_FORMATION('',$,#24139);
#24009=PRODUCT_DEFINITION_FORMATION('',$,#24140);
#24010=PRODUCT_DEFINITION_FORMATION('',$,#24141);
#24011=PRODUCT_DEFINITION_FORMATION('',$,#24142);
#24012=PRODUCT_DEFINITION_FORMATION('',$,#24143);
#24013=PRODUCT_DEFINITION_FORMATION('',$,#24144);
#24014=PRODUCT_DEFINITION_FORMATION('',$,#24145);
#24015=PRODUCT_DEFINITION_FORMATION('',$,#24146);
#24016=PRODUCT_DEFINITION_FORMATION('',$,#24147);
#24017=PRODUCT_DEFINITION_FORMATION('',$,#24148);
#24018=PRODUCT_RELATED_PRODUCT_CATEGORY('PAT-011','PAT-011',(#24085));
#24019=PRODUCT_RELATED_PRODUCT_CATEGORY('Base and guide',
'Base and guide',(#24086));
#24020=PRODUCT_RELATED_PRODUCT_CATEGORY('Base','Base',(#24087));
#24021=PRODUCT_RELATED_PRODUCT_CATEGORY('Foot','Foot',(#24088));
#24022=PRODUCT_RELATED_PRODUCT_CATEGORY('Foot (1)','Foot (1)',(#24089));
#24023=PRODUCT_RELATED_PRODUCT_CATEGORY('Fixed bearing block',
'Fixed bearing block',(#24090));
#24024=PRODUCT_RELATED_PRODUCT_CATEGORY('Input outer spacer',
'Input outer spacer',(#24091));
#24025=PRODUCT_RELATED_PRODUCT_CATEGORY('Input bearing cap',
'Input bearing cap',(#24092));
#24026=PRODUCT_RELATED_PRODUCT_CATEGORY('Input bearing cap (1)',
'Input bearing cap (1)',(#24093));
#24027=PRODUCT_RELATED_PRODUCT_CATEGORY('Screw support','Screw support',
(#24094));
#24028=PRODUCT_RELATED_PRODUCT_CATEGORY('Screw bushing','Screw bushing',
(#24095));
#24029=PRODUCT_RELATED_PRODUCT_CATEGORY('Screw support (1)',
'Screw support (1)',(#24096));
#24030=PRODUCT_RELATED_PRODUCT_CATEGORY('Screw bushing (1)',
'Screw bushing (1)',(#24097));
#24031=PRODUCT_RELATED_PRODUCT_CATEGORY('Force gauge envelope',
'Force gauge envelope',(#24098));
#24032=PRODUCT_RELATED_PRODUCT_CATEGORY('Gauge mounting saddle',
'Gauge mounting saddle',(#24099));
#24033=PRODUCT_RELATED_PRODUCT_CATEGORY(
'Linear Guide Rail - 15 mm, 220 mm Long',
'Linear Guide Rail - 15 mm, 220 mm Long',(#24100));
#24034=PRODUCT_RELATED_PRODUCT_CATEGORY(
'Sealed Ball Bearing - 10 x 30 x 9 mm',
'Sealed Ball Bearing - 10 x 30 x 9 mm',(#24101));
#24035=PRODUCT_RELATED_PRODUCT_CATEGORY('Inner ring','Inner ring',(#24102));
#24036=PRODUCT_RELATED_PRODUCT_CATEGORY('Outer ring','Outer ring',(#24103));
#24037=PRODUCT_RELATED_PRODUCT_CATEGORY('Balls','Balls',(#24104));
#24038=PRODUCT_RELATED_PRODUCT_CATEGORY('Cage','Cage',(#24105));
#24039=PRODUCT_RELATED_PRODUCT_CATEGORY('Seals 2RS','Seals 2RS',(#24106));
#24040=PRODUCT_RELATED_PRODUCT_CATEGORY('Sliding bearing and gauge rod',
'Sliding bearing and gauge rod',(#24107));
#24041=PRODUCT_RELATED_PRODUCT_CATEGORY('Sliding plate','Sliding plate',
(#24108));
#24042=PRODUCT_RELATED_PRODUCT_CATEGORY('Sliding bearing block',
'Sliding bearing block',(#24109));
#24043=PRODUCT_RELATED_PRODUCT_CATEGORY('Output outer spacer',
'Output outer spacer',(#24110));
#24044=PRODUCT_RELATED_PRODUCT_CATEGORY('Output bearing cap',
'Output bearing cap',(#24111));
#24045=PRODUCT_RELATED_PRODUCT_CATEGORY('Output bearing cap (1)',
'Output bearing cap (1)',(#24112));
#24046=PRODUCT_RELATED_PRODUCT_CATEGORY('Adjusting nut pedestal',
'Adjusting nut pedestal',(#24113));
#24047=PRODUCT_RELATED_PRODUCT_CATEGORY('Gauge extension rod',
'Gauge extension rod',(#24114));
#24048=PRODUCT_RELATED_PRODUCT_CATEGORY('Gauge rod bracket',
'Gauge rod bracket',(#24115));
#24049=PRODUCT_RELATED_PRODUCT_CATEGORY(
'Flanged Linear Guide Carriage - 15 mm',
'Flanged Linear Guide Carriage - 15 mm',(#24116));
#24050=PRODUCT_RELATED_PRODUCT_CATEGORY('Block','Block',(#24117));
#24051=PRODUCT_RELATED_PRODUCT_CATEGORY('End cap +','End cap +',(#24118));
#24052=PRODUCT_RELATED_PRODUCT_CATEGORY('End cap','End cap',(#24119));
#24053=PRODUCT_RELATED_PRODUCT_CATEGORY('M5x14 Cap Screw',
'M5x14 Cap Screw',(#24120));
#24054=PRODUCT_RELATED_PRODUCT_CATEGORY(
'Sealed Ball Bearing - 12 x 32 x 10 mm',
'Sealed Ball Bearing - 12 x 32 x 10 mm',(#24121));
#24055=PRODUCT_RELATED_PRODUCT_CATEGORY('Inner ring (1)',
'Inner ring (1)',(#24122));
#24056=PRODUCT_RELATED_PRODUCT_CATEGORY('Outer ring (1)',
'Outer ring (1)',(#24123));
#24057=PRODUCT_RELATED_PRODUCT_CATEGORY('Balls (1)','Balls (1)',(#24124));
#24058=PRODUCT_RELATED_PRODUCT_CATEGORY('Cage (1)','Cage (1)',(#24125));
#24059=PRODUCT_RELATED_PRODUCT_CATEGORY('Seals 2RS (1)','Seals 2RS (1)',
(#24126));
#24060=PRODUCT_RELATED_PRODUCT_CATEGORY('M4x10 Cap Screw',
'M4x10 Cap Screw',(#24127));
#24061=PRODUCT_RELATED_PRODUCT_CATEGORY('Input pulley','Input pulley',(#24128));
#24062=PRODUCT_RELATED_PRODUCT_CATEGORY('Input shaft','Input shaft',(#24129));
#24063=PRODUCT_RELATED_PRODUCT_CATEGORY('Input inner spacer',
'Input inner spacer',(#24130));
#24064=PRODUCT_RELATED_PRODUCT_CATEGORY('Input inner sleeve',
'Input inner sleeve',(#24131));
#24065=PRODUCT_RELATED_PRODUCT_CATEGORY('Input M3 set screw',
'Input M3 set screw',(#24132));
#24066=PRODUCT_RELATED_PRODUCT_CATEGORY('Input M3 set screw (1)',
'Input M3 set screw (1)',(#24133));
#24067=PRODUCT_RELATED_PRODUCT_CATEGORY('Input end keeper',
'Input end keeper',(#24134));
#24068=PRODUCT_RELATED_PRODUCT_CATEGORY(
'Timing Pulley - 2 mm Pitch, 20 Teeth, 8 mm Bore',
'Timing Pulley - 2 mm Pitch, 20 Teeth, 8 mm Bore',(#24135));
#24069=PRODUCT_RELATED_PRODUCT_CATEGORY('Sliding pulley',
'Sliding pulley',(#24136));
#24070=PRODUCT_RELATED_PRODUCT_CATEGORY('Output shaft','Output shaft',(#24137));
#24071=PRODUCT_RELATED_PRODUCT_CATEGORY('Output inner spacer',
'Output inner spacer',(#24138));
#24072=PRODUCT_RELATED_PRODUCT_CATEGORY('Output inner sleeve',
'Output inner sleeve',(#24139));
#24073=PRODUCT_RELATED_PRODUCT_CATEGORY('Output M3 set screw',
'Output M3 set screw',(#24140));
#24074=PRODUCT_RELATED_PRODUCT_CATEGORY('Output M3 set screw (1)',
'Output M3 set screw (1)',(#24141));
#24075=PRODUCT_RELATED_PRODUCT_CATEGORY('Output end keeper',
'Output end keeper',(#24142));
#24076=PRODUCT_RELATED_PRODUCT_CATEGORY(
'Timing Pulley - 2 mm Pitch, 40 Teeth, 12 mm Bore',
'Timing Pulley - 2 mm Pitch, 40 Teeth, 12 mm Bore',(#24143));
#24077=PRODUCT_RELATED_PRODUCT_CATEGORY('Cap Screw - M4x16',
'Cap Screw - M4x16',(#24144));
#24078=PRODUCT_RELATED_PRODUCT_CATEGORY('Adjusting screw',
'Adjusting screw',(#24145));
#24079=PRODUCT_RELATED_PRODUCT_CATEGORY('M8x1.25 adjusting spindle',
'M8x1.25 adjusting spindle',(#24146));
#24080=PRODUCT_RELATED_PRODUCT_CATEGORY('Adjusting knob',
'Adjusting knob',(#24147));
#24081=PRODUCT_RELATED_PRODUCT_CATEGORY('Socket Set Screw - M4x6',
'Socket Set Screw - M4x6',(#24148));
#24082=APPLICATION_PROTOCOL_DEFINITION('international standard',
'automotive_design',2009,#24083);
#24083=APPLICATION_CONTEXT(
'Core Data for Automotive Mechanical Design Process');
#24084=PRODUCT_CONTEXT('part definition',#24083,'mechanical');
#24085=PRODUCT('PAT-011','PAT-011',
'PAT-011',(#24084));
#24086=PRODUCT('Base and guide','Base and guide','Base and guide',(#24084));
#24087=PRODUCT('Base','Base','Base',(#24084));
#24088=PRODUCT('Foot','Foot','Foot',(#24084));
#24089=PRODUCT('Foot (1)','Foot (1)','Foot (1)',(#24084));
#24090=PRODUCT('Fixed bearing block','Fixed bearing block',
'Fixed bearing block',(#24084));
#24091=PRODUCT('Input outer spacer','Input outer spacer',
'Input outer spacer',(#24084));
#24092=PRODUCT('Input bearing cap','Input bearing cap',
'Input bearing cap',(#24084));
#24093=PRODUCT('Input bearing cap (1)','Input bearing cap (1)',
'Input bearing cap (1)',(#24084));
#24094=PRODUCT('Screw support','Screw support','Screw support',(#24084));
#24095=PRODUCT('Screw bushing','Screw bushing','Screw bushing',(#24084));
#24096=PRODUCT('Screw support (1)','Screw support (1)','Screw support (1)',(#24084));
#24097=PRODUCT('Screw bushing (1)','Screw bushing (1)','Screw bushing (1)',(#24084));
#24098=PRODUCT('Force gauge envelope','Force gauge envelope',
'Force gauge envelope',(#24084));
#24099=PRODUCT('Gauge mounting saddle','Gauge mounting saddle',
'Gauge mounting saddle',(#24084));
#24100=PRODUCT('Linear Guide Rail - 15 mm, 220 mm Long',
'Linear Guide Rail - 15 mm, 220 mm Long',
'Linear Guide Rail - 15 mm, 220 mm Long',(#24084));
#24101=PRODUCT('Sealed Ball Bearing - 10 x 30 x 9 mm',
'Sealed Ball Bearing - 10 x 30 x 9 mm',
'Sealed Ball Bearing - 10 x 30 x 9 mm',(#24084));
#24102=PRODUCT('Inner ring','Inner ring','Inner ring',(#24084));
#24103=PRODUCT('Outer ring','Outer ring','Outer ring',(#24084));
#24104=PRODUCT('Balls','Balls','Balls',(#24084));
#24105=PRODUCT('Cage','Cage','Cage',(#24084));
#24106=PRODUCT('Seals 2RS','Seals 2RS','Seals 2RS',(#24084));
#24107=PRODUCT('Sliding bearing and gauge rod',
'Sliding bearing and gauge rod','Sliding bearing and gauge rod',(#24084));
#24108=PRODUCT('Sliding plate','Sliding plate','Sliding plate',(#24084));
#24109=PRODUCT('Sliding bearing block','Sliding bearing block',
'Sliding bearing block',(#24084));
#24110=PRODUCT('Output outer spacer','Output outer spacer',
'Output outer spacer',(#24084));
#24111=PRODUCT('Output bearing cap','Output bearing cap',
'Output bearing cap',(#24084));
#24112=PRODUCT('Output bearing cap (1)','Output bearing cap (1)',
'Output bearing cap (1)',(#24084));
#24113=PRODUCT('Adjusting nut pedestal','Adjusting nut pedestal',
'Adjusting nut pedestal',(#24084));
#24114=PRODUCT('Gauge extension rod','Gauge extension rod',
'Gauge extension rod',(#24084));
#24115=PRODUCT('Gauge rod bracket','Gauge rod bracket',
'Gauge rod bracket',(#24084));
#24116=PRODUCT('Flanged Linear Guide Carriage - 15 mm',
'Flanged Linear Guide Carriage - 15 mm',
'Flanged Linear Guide Carriage - 15 mm',(#24084));
#24117=PRODUCT('Block','Block','Block',(#24084));
#24118=PRODUCT('End cap +','End cap +','End cap +',(#24084));
#24119=PRODUCT('End cap','End cap','End cap',(#24084));
#24120=PRODUCT('M5x14 Cap Screw','M5x14 Cap Screw','M5x14 Cap Screw',(#24084));
#24121=PRODUCT('Sealed Ball Bearing - 12 x 32 x 10 mm',
'Sealed Ball Bearing - 12 x 32 x 10 mm',
'Sealed Ball Bearing - 12 x 32 x 10 mm',(#24084));
#24122=PRODUCT('Inner ring (1)','Inner ring (1)','Inner ring (1)',(#24084));
#24123=PRODUCT('Outer ring (1)','Outer ring (1)','Outer ring (1)',(#24084));
#24124=PRODUCT('Balls (1)','Balls (1)','Balls (1)',(#24084));
#24125=PRODUCT('Cage (1)','Cage (1)','Cage (1)',(#24084));
#24126=PRODUCT('Seals 2RS (1)','Seals 2RS (1)','Seals 2RS (1)',(#24084));
#24127=PRODUCT('M4x10 Cap Screw','M4x10 Cap Screw','M4x10 Cap Screw',(#24084));
#24128=PRODUCT('Input pulley','Input pulley','Input pulley',(#24084));
#24129=PRODUCT('Input shaft','Input shaft','Input shaft',(#24084));
#24130=PRODUCT('Input inner spacer','Input inner spacer',
'Input inner spacer',(#24084));
#24131=PRODUCT('Input inner sleeve','Input inner sleeve',
'Input inner sleeve',(#24084));
#24132=PRODUCT('Input M3 set screw','Input M3 set screw',
'Input M3 set screw',(#24084));
#24133=PRODUCT('Input M3 set screw (1)','Input M3 set screw (1)',
'Input M3 set screw (1)',(#24084));
#24134=PRODUCT('Input end keeper','Input end keeper','Input end keeper',
(#24084));
#24135=PRODUCT('Timing Pulley - 2 mm Pitch, 20 Teeth, 8 mm Bore',
'Timing Pulley - 2 mm Pitch, 20 Teeth, 8 mm Bore',
'Timing Pulley - 2 mm Pitch, 20 Teeth, 8 mm Bore',(#24084));
#24136=PRODUCT('Sliding pulley','Sliding pulley','Sliding pulley',(#24084));
#24137=PRODUCT('Output shaft','Output shaft','Output shaft',(#24084));
#24138=PRODUCT('Output inner spacer','Output inner spacer',
'Output inner spacer',(#24084));
#24139=PRODUCT('Output inner sleeve','Output inner sleeve',
'Output inner sleeve',(#24084));
#24140=PRODUCT('Output M3 set screw','Output M3 set screw',
'Output M3 set screw',(#24084));
#24141=PRODUCT('Output M3 set screw (1)','Output M3 set screw (1)',
'Output M3 set screw (1)',(#24084));
#24142=PRODUCT('Output end keeper','Output end keeper',
'Output end keeper',(#24084));
#24143=PRODUCT('Timing Pulley - 2 mm Pitch, 40 Teeth, 12 mm Bore',
'Timing Pulley - 2 mm Pitch, 40 Teeth, 12 mm Bore',
'Timing Pulley - 2 mm Pitch, 40 Teeth, 12 mm Bore',(#24084));
#24144=PRODUCT('Cap Screw - M4x16','Cap Screw - M4x16',
'Cap Screw - M4x16',(#24084));
#24145=PRODUCT('Adjusting screw','Adjusting screw','Adjusting screw',(#24084));
#24146=PRODUCT('M8x1.25 adjusting spindle','M8x1.25 adjusting spindle',
'M8x1.25 adjusting spindle',(#24084));
#24147=PRODUCT('Adjusting knob','Adjusting knob','Adjusting knob',(#24084));
#24148=PRODUCT('Socket Set Screw - M4x6','Socket Set Screw - M4x6',
'Socket Set Screw - M4x6',(#24084));
#24149=PRESENTATION_STYLE_ASSIGNMENT((#24154));
#24150=PRESENTATION_STYLE_ASSIGNMENT((#24155));
#24151=PRESENTATION_STYLE_ASSIGNMENT((#24156));
#24152=PRESENTATION_STYLE_ASSIGNMENT((#24157));
#24153=PRESENTATION_STYLE_ASSIGNMENT((#24158));
#24154=SURFACE_STYLE_USAGE(.BOTH.,#24159);
#24155=SURFACE_STYLE_USAGE(.BOTH.,#24160);
#24156=SURFACE_STYLE_USAGE(.BOTH.,#24161);
#24157=SURFACE_STYLE_USAGE(.BOTH.,#24162);
#24158=SURFACE_STYLE_USAGE(.BOTH.,#24163);
#24159=SURFACE_SIDE_STYLE('',(#24164));
#24160=SURFACE_SIDE_STYLE('',(#24165));
#24161=SURFACE_SIDE_STYLE('',(#24166));
#24162=SURFACE_SIDE_STYLE('',(#24167));
#24163=SURFACE_SIDE_STYLE('',(#24168));
#24164=SURFACE_STYLE_FILL_AREA(#24169);
#24165=SURFACE_STYLE_FILL_AREA(#24170);
#24166=SURFACE_STYLE_FILL_AREA(#24171);
#24167=SURFACE_STYLE_FILL_AREA(#24172);
#24168=SURFACE_STYLE_FILL_AREA(#24173);
#24169=FILL_AREA_STYLE('Steel - Satin',(#24174));
#24170=FILL_AREA_STYLE('CAD Library Painted - Deep blue',(#24175));
#24171=FILL_AREA_STYLE('CAD Library Painted - Steel gray',(#24176));
#24172=FILL_AREA_STYLE('CAD Library Painted - Graphite',(#24177));
#24173=FILL_AREA_STYLE('CAD Library Painted - Engineering blue',(#24178));
#24174=FILL_AREA_STYLE_COLOUR('Steel - Satin',#24179);
#24175=FILL_AREA_STYLE_COLOUR('CAD Library Painted - Deep blue',#24180);
#24176=FILL_AREA_STYLE_COLOUR('CAD Library Painted - Steel gray',#24181);
#24177=FILL_AREA_STYLE_COLOUR('CAD Library Painted - Graphite',#24182);
#24178=FILL_AREA_STYLE_COLOUR('CAD Library Painted - Engineering blue',
#24183);
#24179=COLOUR_RGB('Steel - Satin',0.627450980392157,0.627450980392157,0.627450980392157);
#24180=COLOUR_RGB('CAD Library Painted - Deep blue',0.0784313725490196,
0.203921568627451,0.349019607843137);
#24181=COLOUR_RGB('CAD Library Painted - Steel gray',0.592156862745098,
0.631372549019608,0.67843137254902);
#24182=COLOUR_RGB('CAD Library Painted - Graphite',0.168627450980392,0.192156862745098,
0.231372549019608);
#24183=COLOUR_RGB('CAD Library Painted - Engineering blue',0.12156862745098,
0.356862745098039,0.6);
#24184=COLOUR_RGB('Dark Blue',0.08,0.2,0.34);
#24185=FILL_AREA_STYLE_COLOUR('',#24184);
#24186=FILL_AREA_STYLE('',(#24185));
#24187=SURFACE_STYLE_FILL_AREA(#24186);
#24188=SURFACE_SIDE_STYLE('',(#24187));
#24189=SURFACE_STYLE_USAGE(.BOTH.,#24188);
#24190=PRESENTATION_STYLE_ASSIGNMENT((#24189));
#24191=COLOUR_RGB('Light Blue',0.38,0.62,0.78);
#24192=FILL_AREA_STYLE_COLOUR('',#24191);
#24193=FILL_AREA_STYLE('',(#24192));
#24194=SURFACE_STYLE_FILL_AREA(#24193);
#24195=SURFACE_SIDE_STYLE('',(#24194));
#24196=SURFACE_STYLE_USAGE(.BOTH.,#24195);
#24197=PRESENTATION_STYLE_ASSIGNMENT((#24196));
#24198=COLOUR_RGB('Sky Blue',0.24,0.69,0.87);
#24199=FILL_AREA_STYLE_COLOUR('',#24198);
#24200=FILL_AREA_STYLE('',(#24199));
#24201=SURFACE_STYLE_FILL_AREA(#24200);
#24202=SURFACE_SIDE_STYLE('',(#24201));
#24203=SURFACE_STYLE_USAGE(.BOTH.,#24202);
#24204=PRESENTATION_STYLE_ASSIGNMENT((#24203));
#24205=COLOUR_RGB('Grey',0.48,0.52,0.57);
#24206=FILL_AREA_STYLE_COLOUR('',#24205);
#24207=FILL_AREA_STYLE('',(#24206));
#24208=SURFACE_STYLE_FILL_AREA(#24207);
#24209=SURFACE_SIDE_STYLE('',(#24208));
#24210=SURFACE_STYLE_USAGE(.BOTH.,#24209);
#24211=PRESENTATION_STYLE_ASSIGNMENT((#24210));
#24212=COLOUR_RGB('Black',0.12,0.14,0.17);
#24213=FILL_AREA_STYLE_COLOUR('',#24212);
#24214=FILL_AREA_STYLE('',(#24213));
#24215=SURFACE_STYLE_FILL_AREA(#24214);
#24216=SURFACE_SIDE_STYLE('',(#24215));
#24217=SURFACE_STYLE_USAGE(.BOTH.,#24216);
#24218=PRESENTATION_STYLE_ASSIGNMENT((#24217));
#24219=COLOUR_RGB('Off White',0.89,0.88,0.83);
#24220=FILL_AREA_STYLE_COLOUR('',#24219);
#24221=FILL_AREA_STYLE('',(#24220));
#24222=SURFACE_STYLE_FILL_AREA(#24221);
#24223=SURFACE_SIDE_STYLE('',(#24222));
#24224=SURFACE_STYLE_USAGE(.BOTH.,#24223);
#24225=PRESENTATION_STYLE_ASSIGNMENT((#24224));
ENDSEC;
END-ISO-10303-21;
